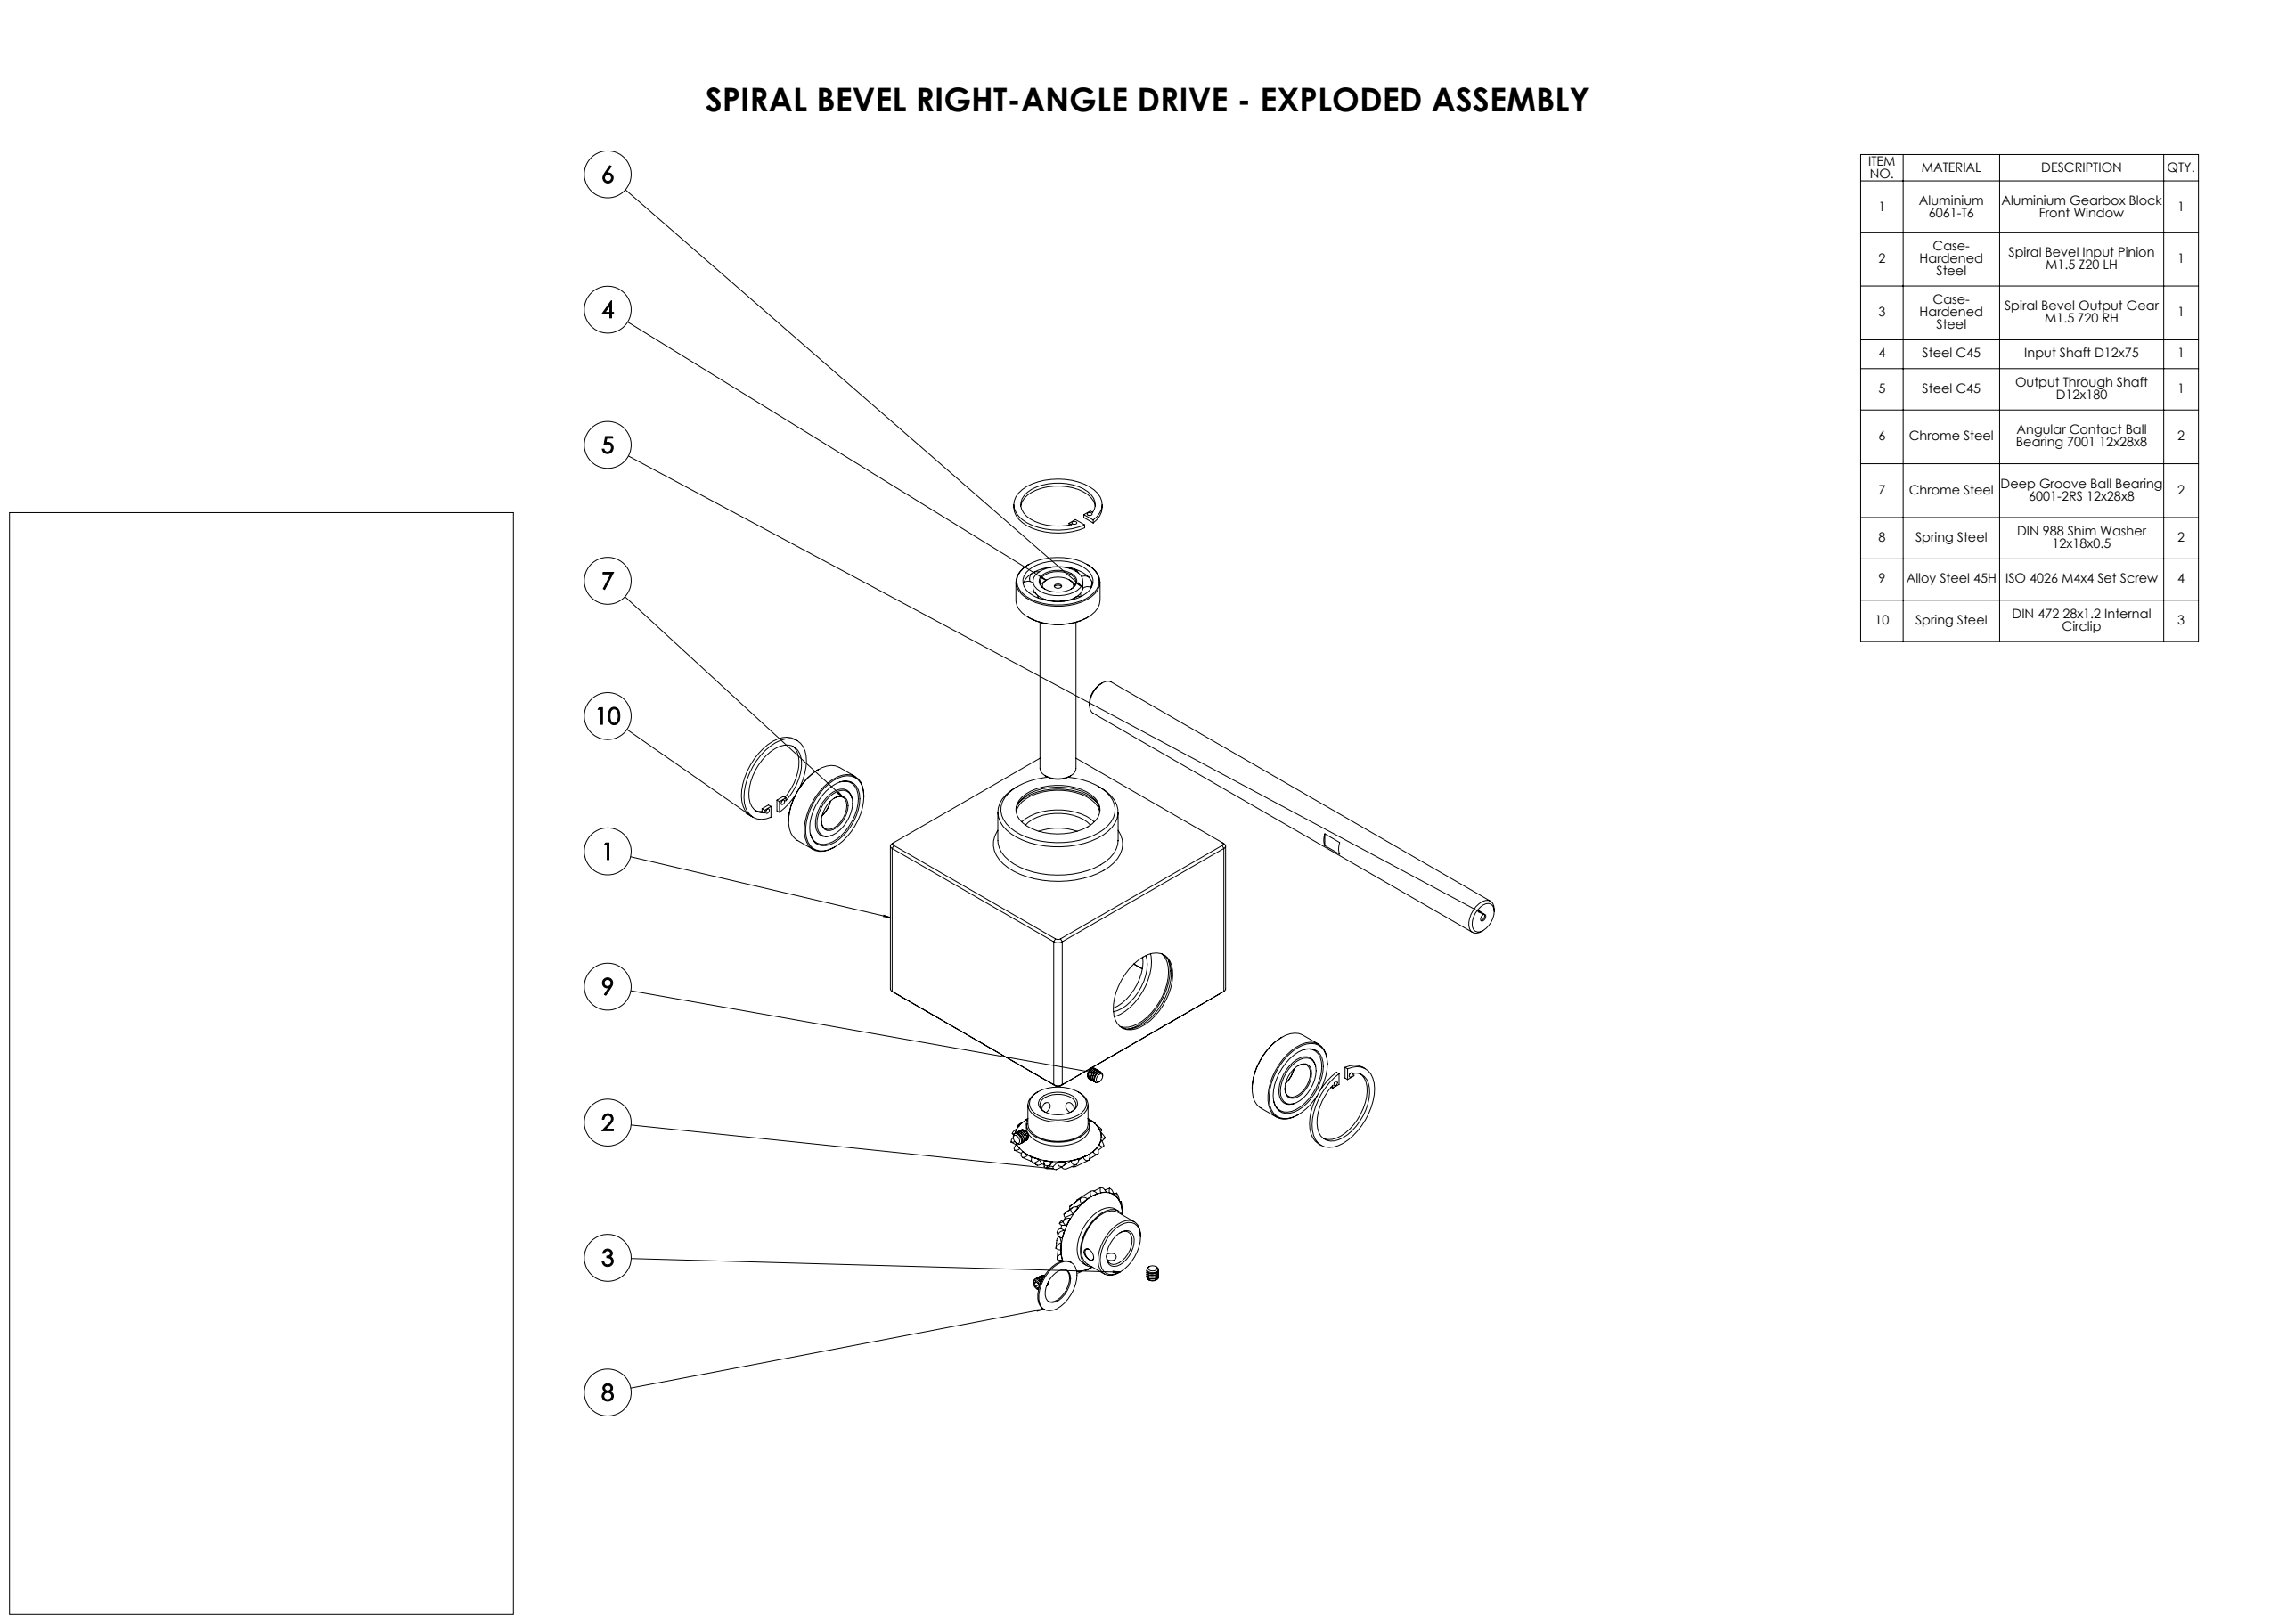
ISO-10303-21;
HEADER;
/* Generated by software containing ST-Developer
 * from STEP Tools, Inc. (www.steptools.com) 
 */

FILE_DESCRIPTION(
/* description */ (''),
/* implementation_level */ '2;1');

FILE_NAME(
/* name */ 'MAS-365',
/* time_stamp */ '2026-10-11T09:12:28-07:00',
/* author */ (''),
/* organization */ (''),
/* preprocessor_version */ 'ST-DEVELOPER v20.2',
/* originating_system */ 'Autodesk Translation Framework v15.15.0.0',
/* authorisation */ '');

FILE_SCHEMA (('AUTOMOTIVE_DESIGN { 1 0 10303 214 3 1 1 }'));
ENDSEC;

DATA;
#10=MECHANICAL_DESIGN_GEOMETRIC_PRESENTATION_REPRESENTATION('',(#647,#648,
#649,#650,#651,#652,#653,#654,#655,#656),#23254);
#11=ITEM_DEFINED_TRANSFORMATION($,$,#7147,#7813);
#12=ITEM_DEFINED_TRANSFORMATION($,$,#7279,#7814);
#13=ITEM_DEFINED_TRANSFORMATION($,$,#7412,#7815);
#14=ITEM_DEFINED_TRANSFORMATION($,$,#7544,#7816);
#15=ITEM_DEFINED_TRANSFORMATION($,$,#7574,#7817);
#16=ITEM_DEFINED_TRANSFORMATION($,$,#7604,#7818);
#17=ITEM_DEFINED_TRANSFORMATION($,$,#7604,#7819);
#18=ITEM_DEFINED_TRANSFORMATION($,$,#7713,#7820);
#19=ITEM_DEFINED_TRANSFORMATION($,$,#7713,#7821);
#20=ITEM_DEFINED_TRANSFORMATION($,$,#7746,#7822);
#21=ITEM_DEFINED_TRANSFORMATION($,$,#7746,#7823);
#22=ITEM_DEFINED_TRANSFORMATION($,$,#7755,#7824);
#23=ITEM_DEFINED_TRANSFORMATION($,$,#7755,#7825);
#24=ITEM_DEFINED_TRANSFORMATION($,$,#7755,#7826);
#25=ITEM_DEFINED_TRANSFORMATION($,$,#7755,#7827);
#26=ITEM_DEFINED_TRANSFORMATION($,$,#7792,#7828);
#27=ITEM_DEFINED_TRANSFORMATION($,$,#7792,#7829);
#28=ITEM_DEFINED_TRANSFORMATION($,$,#7792,#7830);
#29=(
REPRESENTATION_RELATIONSHIP($,$,#23300,#23299)
REPRESENTATION_RELATIONSHIP_WITH_TRANSFORMATION(#11)
SHAPE_REPRESENTATION_RELATIONSHIP()
);
#30=(
REPRESENTATION_RELATIONSHIP($,$,#23301,#23299)
REPRESENTATION_RELATIONSHIP_WITH_TRANSFORMATION(#12)
SHAPE_REPRESENTATION_RELATIONSHIP()
);
#31=(
REPRESENTATION_RELATIONSHIP($,$,#23302,#23299)
REPRESENTATION_RELATIONSHIP_WITH_TRANSFORMATION(#13)
SHAPE_REPRESENTATION_RELATIONSHIP()
);
#32=(
REPRESENTATION_RELATIONSHIP($,$,#23303,#23299)
REPRESENTATION_RELATIONSHIP_WITH_TRANSFORMATION(#14)
SHAPE_REPRESENTATION_RELATIONSHIP()
);
#33=(
REPRESENTATION_RELATIONSHIP($,$,#23304,#23299)
REPRESENTATION_RELATIONSHIP_WITH_TRANSFORMATION(#15)
SHAPE_REPRESENTATION_RELATIONSHIP()
);
#34=(
REPRESENTATION_RELATIONSHIP($,$,#23305,#23299)
REPRESENTATION_RELATIONSHIP_WITH_TRANSFORMATION(#16)
SHAPE_REPRESENTATION_RELATIONSHIP()
);
#35=(
REPRESENTATION_RELATIONSHIP($,$,#23305,#23299)
REPRESENTATION_RELATIONSHIP_WITH_TRANSFORMATION(#17)
SHAPE_REPRESENTATION_RELATIONSHIP()
);
#36=(
REPRESENTATION_RELATIONSHIP($,$,#23306,#23299)
REPRESENTATION_RELATIONSHIP_WITH_TRANSFORMATION(#18)
SHAPE_REPRESENTATION_RELATIONSHIP()
);
#37=(
REPRESENTATION_RELATIONSHIP($,$,#23306,#23299)
REPRESENTATION_RELATIONSHIP_WITH_TRANSFORMATION(#19)
SHAPE_REPRESENTATION_RELATIONSHIP()
);
#38=(
REPRESENTATION_RELATIONSHIP($,$,#23307,#23299)
REPRESENTATION_RELATIONSHIP_WITH_TRANSFORMATION(#20)
SHAPE_REPRESENTATION_RELATIONSHIP()
);
#39=(
REPRESENTATION_RELATIONSHIP($,$,#23307,#23299)
REPRESENTATION_RELATIONSHIP_WITH_TRANSFORMATION(#21)
SHAPE_REPRESENTATION_RELATIONSHIP()
);
#40=(
REPRESENTATION_RELATIONSHIP($,$,#23308,#23299)
REPRESENTATION_RELATIONSHIP_WITH_TRANSFORMATION(#22)
SHAPE_REPRESENTATION_RELATIONSHIP()
);
#41=(
REPRESENTATION_RELATIONSHIP($,$,#23308,#23299)
REPRESENTATION_RELATIONSHIP_WITH_TRANSFORMATION(#23)
SHAPE_REPRESENTATION_RELATIONSHIP()
);
#42=(
REPRESENTATION_RELATIONSHIP($,$,#23308,#23299)
REPRESENTATION_RELATIONSHIP_WITH_TRANSFORMATION(#24)
SHAPE_REPRESENTATION_RELATIONSHIP()
);
#43=(
REPRESENTATION_RELATIONSHIP($,$,#23308,#23299)
REPRESENTATION_RELATIONSHIP_WITH_TRANSFORMATION(#25)
SHAPE_REPRESENTATION_RELATIONSHIP()
);
#44=(
REPRESENTATION_RELATIONSHIP($,$,#23309,#23299)
REPRESENTATION_RELATIONSHIP_WITH_TRANSFORMATION(#26)
SHAPE_REPRESENTATION_RELATIONSHIP()
);
#45=(
REPRESENTATION_RELATIONSHIP($,$,#23309,#23299)
REPRESENTATION_RELATIONSHIP_WITH_TRANSFORMATION(#27)
SHAPE_REPRESENTATION_RELATIONSHIP()
);
#46=(
REPRESENTATION_RELATIONSHIP($,$,#23309,#23299)
REPRESENTATION_RELATIONSHIP_WITH_TRANSFORMATION(#28)
SHAPE_REPRESENTATION_RELATIONSHIP()
);
#47=CONTEXT_DEPENDENT_SHAPE_REPRESENTATION(#29,#23281);
#48=CONTEXT_DEPENDENT_SHAPE_REPRESENTATION(#30,#23282);
#49=CONTEXT_DEPENDENT_SHAPE_REPRESENTATION(#31,#23283);
#50=CONTEXT_DEPENDENT_SHAPE_REPRESENTATION(#32,#23284);
#51=CONTEXT_DEPENDENT_SHAPE_REPRESENTATION(#33,#23285);
#52=CONTEXT_DEPENDENT_SHAPE_REPRESENTATION(#34,#23286);
#53=CONTEXT_DEPENDENT_SHAPE_REPRESENTATION(#35,#23287);
#54=CONTEXT_DEPENDENT_SHAPE_REPRESENTATION(#36,#23288);
#55=CONTEXT_DEPENDENT_SHAPE_REPRESENTATION(#37,#23289);
#56=CONTEXT_DEPENDENT_SHAPE_REPRESENTATION(#38,#23290);
#57=CONTEXT_DEPENDENT_SHAPE_REPRESENTATION(#39,#23291);
#58=CONTEXT_DEPENDENT_SHAPE_REPRESENTATION(#40,#23292);
#59=CONTEXT_DEPENDENT_SHAPE_REPRESENTATION(#41,#23293);
#60=CONTEXT_DEPENDENT_SHAPE_REPRESENTATION(#42,#23294);
#61=CONTEXT_DEPENDENT_SHAPE_REPRESENTATION(#43,#23295);
#62=CONTEXT_DEPENDENT_SHAPE_REPRESENTATION(#44,#23296);
#63=CONTEXT_DEPENDENT_SHAPE_REPRESENTATION(#45,#23297);
#64=CONTEXT_DEPENDENT_SHAPE_REPRESENTATION(#46,#23298);
#65=NEXT_ASSEMBLY_USAGE_OCCURRENCE(
'01_Aluminium_Gearbox_Block_Front_Window:2',
'01_Aluminium_Gearbox_Block_Front_Window:2',
'01_Aluminium_Gearbox_Block_Front_Window:2',#23311,#23312,
'01_Aluminium_Gearbox_Block_Front_Window:2');
#66=NEXT_ASSEMBLY_USAGE_OCCURRENCE(
'02_Spiral_Bevel_Input_Pinion_M1.5_Z20_LH:2',
'02_Spiral_Bevel_Input_Pinion_M1.5_Z20_LH:2',
'02_Spiral_Bevel_Input_Pinion_M1.5_Z20_LH:2',#23311,#23313,
'02_Spiral_Bevel_Input_Pinion_M1.5_Z20_LH:2');
#67=NEXT_ASSEMBLY_USAGE_OCCURRENCE(
'03_Spiral_Bevel_Output_Gear_M1.5_Z20_RH:2',
'03_Spiral_Bevel_Output_Gear_M1.5_Z20_RH:2',
'03_Spiral_Bevel_Output_Gear_M1.5_Z20_RH:2',#23311,#23314,
'03_Spiral_Bevel_Output_Gear_M1.5_Z20_RH:2');
#68=NEXT_ASSEMBLY_USAGE_OCCURRENCE('04_Input_Shaft_D12x75:2',
'04_Input_Shaft_D12x75:2','04_Input_Shaft_D12x75:2',#23311,#23315,
'04_Input_Shaft_D12x75:2');
#69=NEXT_ASSEMBLY_USAGE_OCCURRENCE('05_Output_Through_Shaft_D12x180:2',
'05_Output_Through_Shaft_D12x180:2','05_Output_Through_Shaft_D12x180:2',
#23311,#23316,'05_Output_Through_Shaft_D12x180:2');
#70=NEXT_ASSEMBLY_USAGE_OCCURRENCE(
'06_Angular_Contact_Ball_Bearing_7001_12x28x8:2',
'06_Angular_Contact_Ball_Bearing_7001_12x28x8:2',
'06_Angular_Contact_Ball_Bearing_7001_12x28x8:2',#23311,#23317,
'06_Angular_Contact_Ball_Bearing_7001_12x28x8:2');
#71=NEXT_ASSEMBLY_USAGE_OCCURRENCE(
'06_Angular_Contact_Ball_Bearing_7001_12x28x8:3',
'06_Angular_Contact_Ball_Bearing_7001_12x28x8:3',
'06_Angular_Contact_Ball_Bearing_7001_12x28x8:3',#23311,#23317,
'06_Angular_Contact_Ball_Bearing_7001_12x28x8:3');
#72=NEXT_ASSEMBLY_USAGE_OCCURRENCE(
'07_Deep_Groove_Ball_Bearing_6001-2RS_12x28x8:2',
'07_Deep_Groove_Ball_Bearing_6001-2RS_12x28x8:2',
'07_Deep_Groove_Ball_Bearing_6001-2RS_12x28x8:2',#23311,#23318,
'07_Deep_Groove_Ball_Bearing_6001-2RS_12x28x8:2');
#73=NEXT_ASSEMBLY_USAGE_OCCURRENCE(
'07_Deep_Groove_Ball_Bearing_6001-2RS_12x28x8:3',
'07_Deep_Groove_Ball_Bearing_6001-2RS_12x28x8:3',
'07_Deep_Groove_Ball_Bearing_6001-2RS_12x28x8:3',#23311,#23318,
'07_Deep_Groove_Ball_Bearing_6001-2RS_12x28x8:3');
#74=NEXT_ASSEMBLY_USAGE_OCCURRENCE('08_DIN_988_Shim_Washer_12x18x0.5:2',
'08_DIN_988_Shim_Washer_12x18x0.5:2',
'08_DIN_988_Shim_Washer_12x18x0.5:2',#23311,#23319,
'08_DIN_988_Shim_Washer_12x18x0.5:2');
#75=NEXT_ASSEMBLY_USAGE_OCCURRENCE('08_DIN_988_Shim_Washer_12x18x0.5:3',
'08_DIN_988_Shim_Washer_12x18x0.5:3',
'08_DIN_988_Shim_Washer_12x18x0.5:3',#23311,#23319,
'08_DIN_988_Shim_Washer_12x18x0.5:3');
#76=NEXT_ASSEMBLY_USAGE_OCCURRENCE('09_ISO_4026_M4x4_Set_Screw:2',
'09_ISO_4026_M4x4_Set_Screw:2','09_ISO_4026_M4x4_Set_Screw:2',#23311,#23320,
'09_ISO_4026_M4x4_Set_Screw:2');
#77=NEXT_ASSEMBLY_USAGE_OCCURRENCE('09_ISO_4026_M4x4_Set_Screw:3',
'09_ISO_4026_M4x4_Set_Screw:3','09_ISO_4026_M4x4_Set_Screw:3',#23311,#23320,
'09_ISO_4026_M4x4_Set_Screw:3');
#78=NEXT_ASSEMBLY_USAGE_OCCURRENCE('09_ISO_4026_M4x4_Set_Screw:4',
'09_ISO_4026_M4x4_Set_Screw:4','09_ISO_4026_M4x4_Set_Screw:4',#23311,#23320,
'09_ISO_4026_M4x4_Set_Screw:4');
#79=NEXT_ASSEMBLY_USAGE_OCCURRENCE('09_ISO_4026_M4x4_Set_Screw:5',
'09_ISO_4026_M4x4_Set_Screw:5','09_ISO_4026_M4x4_Set_Screw:5',#23311,#23320,
'09_ISO_4026_M4x4_Set_Screw:5');
#80=NEXT_ASSEMBLY_USAGE_OCCURRENCE(
'10_DIN_472_28x1.2_Internal_Circlip:2',
'10_DIN_472_28x1.2_Internal_Circlip:2',
'10_DIN_472_28x1.2_Internal_Circlip:2',#23311,#23321,
'10_DIN_472_28x1.2_Internal_Circlip:2');
#81=NEXT_ASSEMBLY_USAGE_OCCURRENCE(
'10_DIN_472_28x1.2_Internal_Circlip:3',
'10_DIN_472_28x1.2_Internal_Circlip:3',
'10_DIN_472_28x1.2_Internal_Circlip:3',#23311,#23321,
'10_DIN_472_28x1.2_Internal_Circlip:3');
#82=NEXT_ASSEMBLY_USAGE_OCCURRENCE(
'10_DIN_472_28x1.2_Internal_Circlip:4',
'10_DIN_472_28x1.2_Internal_Circlip:4',
'10_DIN_472_28x1.2_Internal_Circlip:4',#23311,#23321,
'10_DIN_472_28x1.2_Internal_Circlip:4');
#83=SPHERICAL_SURFACE('',#7605,2.38125);
#84=SPHERICAL_SURFACE('',#7635,2.38125);
#85=SPHERICAL_SURFACE('',#7641,2.38125);
#86=SPHERICAL_SURFACE('',#7647,2.38125);
#87=SPHERICAL_SURFACE('',#7653,2.38125);
#88=SPHERICAL_SURFACE('',#7659,2.38125);
#89=SPHERICAL_SURFACE('',#7665,2.38125);
#90=SPHERICAL_SURFACE('',#7671,2.38125);
#91=SPHERICAL_SURFACE('',#7677,2.38125);
#92=SPHERICAL_SURFACE('',#7689,2.38125);
#93=B_SPLINE_SURFACE_WITH_KNOTS('',3,3,((#12095,#12096,#12097,#12098),(#12099,
#12100,#12101,#12102),(#12103,#12104,#12105,#12106),(#12107,#12108,#12109,
#12110),(#12111,#12112,#12113,#12114),(#12115,#12116,#12117,#12118)),
 .UNSPECIFIED.,.F.,.F.,.F.,(4,1,1,4),(4,4),(0.,0.285714285714286,0.571428571428571,
1.),(0.,1.),.UNSPECIFIED.);
#94=B_SPLINE_SURFACE_WITH_KNOTS('',3,3,((#12155,#12156,#12157,#12158),(#12159,
#12160,#12161,#12162),(#12163,#12164,#12165,#12166),(#12167,#12168,#12169,
#12170),(#12171,#12172,#12173,#12174),(#12175,#12176,#12177,#12178)),
 .UNSPECIFIED.,.F.,.F.,.F.,(4,1,1,4),(4,4),(0.,0.285714285714286,0.571428571428571,
1.),(0.,1.),.UNSPECIFIED.);
#95=B_SPLINE_SURFACE_WITH_KNOTS('',3,3,((#12215,#12216,#12217,#12218),(#12219,
#12220,#12221,#12222),(#12223,#12224,#12225,#12226),(#12227,#12228,#12229,
#12230),(#12231,#12232,#12233,#12234),(#12235,#12236,#12237,#12238)),
 .UNSPECIFIED.,.F.,.F.,.F.,(4,1,1,4),(4,4),(0.,0.285714285714286,0.571428571428571,
1.),(0.,1.),.UNSPECIFIED.);
#96=B_SPLINE_SURFACE_WITH_KNOTS('',3,3,((#12275,#12276,#12277,#12278),(#12279,
#12280,#12281,#12282),(#12283,#12284,#12285,#12286),(#12287,#12288,#12289,
#12290),(#12291,#12292,#12293,#12294),(#12295,#12296,#12297,#12298)),
 .UNSPECIFIED.,.F.,.F.,.F.,(4,1,1,4),(4,4),(0.,0.285714285714286,0.571428571428571,
1.),(0.,1.),.UNSPECIFIED.);
#97=B_SPLINE_SURFACE_WITH_KNOTS('',3,3,((#12335,#12336,#12337,#12338),(#12339,
#12340,#12341,#12342),(#12343,#12344,#12345,#12346),(#12347,#12348,#12349,
#12350),(#12351,#12352,#12353,#12354),(#12355,#12356,#12357,#12358)),
 .UNSPECIFIED.,.F.,.F.,.F.,(4,1,1,4),(4,4),(0.,0.285714285714286,0.571428571428571,
1.),(0.,1.),.UNSPECIFIED.);
#98=B_SPLINE_SURFACE_WITH_KNOTS('',3,3,((#12395,#12396,#12397,#12398),(#12399,
#12400,#12401,#12402),(#12403,#12404,#12405,#12406),(#12407,#12408,#12409,
#12410),(#12411,#12412,#12413,#12414),(#12415,#12416,#12417,#12418)),
 .UNSPECIFIED.,.F.,.F.,.F.,(4,1,1,4),(4,4),(0.,0.285714285714286,0.571428571428571,
1.),(0.,1.),.UNSPECIFIED.);
#99=B_SPLINE_SURFACE_WITH_KNOTS('',3,3,((#12455,#12456,#12457,#12458),(#12459,
#12460,#12461,#12462),(#12463,#12464,#12465,#12466),(#12467,#12468,#12469,
#12470),(#12471,#12472,#12473,#12474),(#12475,#12476,#12477,#12478)),
 .UNSPECIFIED.,.F.,.F.,.F.,(4,1,1,4),(4,4),(0.,0.285714285714286,0.571428571428571,
1.),(0.,1.),.UNSPECIFIED.);
#100=B_SPLINE_SURFACE_WITH_KNOTS('',3,3,((#12515,#12516,#12517,#12518),
(#12519,#12520,#12521,#12522),(#12523,#12524,#12525,#12526),(#12527,#12528,
#12529,#12530),(#12531,#12532,#12533,#12534),(#12535,#12536,#12537,#12538)),
 .UNSPECIFIED.,.F.,.F.,.F.,(4,1,1,4),(4,4),(0.,0.285714285714286,0.571428571428571,
1.),(0.,1.),.UNSPECIFIED.);
#101=B_SPLINE_SURFACE_WITH_KNOTS('',3,3,((#12575,#12576,#12577,#12578),
(#12579,#12580,#12581,#12582),(#12583,#12584,#12585,#12586),(#12587,#12588,
#12589,#12590),(#12591,#12592,#12593,#12594),(#12595,#12596,#12597,#12598)),
 .UNSPECIFIED.,.F.,.F.,.F.,(4,1,1,4),(4,4),(0.,0.285714285714286,0.571428571428571,
1.),(0.,1.),.UNSPECIFIED.);
#102=B_SPLINE_SURFACE_WITH_KNOTS('',3,3,((#12635,#12636,#12637,#12638),
(#12639,#12640,#12641,#12642),(#12643,#12644,#12645,#12646),(#12647,#12648,
#12649,#12650),(#12651,#12652,#12653,#12654),(#12655,#12656,#12657,#12658)),
 .UNSPECIFIED.,.F.,.F.,.F.,(4,1,1,4),(4,4),(0.,0.285714285714286,0.571428571428571,
1.),(0.,1.),.UNSPECIFIED.);
#103=B_SPLINE_SURFACE_WITH_KNOTS('',3,3,((#12695,#12696,#12697,#12698),
(#12699,#12700,#12701,#12702),(#12703,#12704,#12705,#12706),(#12707,#12708,
#12709,#12710),(#12711,#12712,#12713,#12714),(#12715,#12716,#12717,#12718)),
 .UNSPECIFIED.,.F.,.F.,.F.,(4,1,1,4),(4,4),(0.,0.285714285714286,0.571428571428571,
1.),(0.,1.),.UNSPECIFIED.);
#104=B_SPLINE_SURFACE_WITH_KNOTS('',3,3,((#12731,#12732,#12733,#12734),
(#12735,#12736,#12737,#12738),(#12739,#12740,#12741,#12742),(#12743,#12744,
#12745,#12746),(#12747,#12748,#12749,#12750),(#12751,#12752,#12753,#12754)),
 .UNSPECIFIED.,.F.,.F.,.F.,(4,1,1,4),(4,4),(0.,0.285714285714286,0.571428571428571,
1.),(0.,1.),.UNSPECIFIED.);
#105=B_SPLINE_SURFACE_WITH_KNOTS('',3,3,((#12791,#12792,#12793,#12794),
(#12795,#12796,#12797,#12798),(#12799,#12800,#12801,#12802),(#12803,#12804,
#12805,#12806),(#12807,#12808,#12809,#12810),(#12811,#12812,#12813,#12814)),
 .UNSPECIFIED.,.F.,.F.,.F.,(4,1,1,4),(4,4),(0.,0.285714285714286,0.571428571428571,
1.),(0.,1.),.UNSPECIFIED.);
#106=B_SPLINE_SURFACE_WITH_KNOTS('',3,3,((#12851,#12852,#12853,#12854),
(#12855,#12856,#12857,#12858),(#12859,#12860,#12861,#12862),(#12863,#12864,
#12865,#12866),(#12867,#12868,#12869,#12870),(#12871,#12872,#12873,#12874)),
 .UNSPECIFIED.,.F.,.F.,.F.,(4,1,1,4),(4,4),(0.,0.285714285714286,0.571428571428571,
1.),(0.,1.),.UNSPECIFIED.);
#107=B_SPLINE_SURFACE_WITH_KNOTS('',3,3,((#12911,#12912,#12913,#12914),
(#12915,#12916,#12917,#12918),(#12919,#12920,#12921,#12922),(#12923,#12924,
#12925,#12926),(#12927,#12928,#12929,#12930),(#12931,#12932,#12933,#12934)),
 .UNSPECIFIED.,.F.,.F.,.F.,(4,1,1,4),(4,4),(0.,0.285714285714286,0.571428571428571,
1.),(0.,1.),.UNSPECIFIED.);
#108=B_SPLINE_SURFACE_WITH_KNOTS('',3,3,((#12971,#12972,#12973,#12974),
(#12975,#12976,#12977,#12978),(#12979,#12980,#12981,#12982),(#12983,#12984,
#12985,#12986),(#12987,#12988,#12989,#12990),(#12991,#12992,#12993,#12994)),
 .UNSPECIFIED.,.F.,.F.,.F.,(4,1,1,4),(4,4),(0.,0.285714285714286,0.571428571428571,
1.),(0.,1.),.UNSPECIFIED.);
#109=B_SPLINE_SURFACE_WITH_KNOTS('',3,3,((#13031,#13032,#13033,#13034),
(#13035,#13036,#13037,#13038),(#13039,#13040,#13041,#13042),(#13043,#13044,
#13045,#13046),(#13047,#13048,#13049,#13050),(#13051,#13052,#13053,#13054)),
 .UNSPECIFIED.,.F.,.F.,.F.,(4,1,1,4),(4,4),(0.,0.285714285714286,0.571428571428571,
1.),(0.,1.),.UNSPECIFIED.);
#110=B_SPLINE_SURFACE_WITH_KNOTS('',3,3,((#13091,#13092,#13093,#13094),
(#13095,#13096,#13097,#13098),(#13099,#13100,#13101,#13102),(#13103,#13104,
#13105,#13106),(#13107,#13108,#13109,#13110),(#13111,#13112,#13113,#13114)),
 .UNSPECIFIED.,.F.,.F.,.F.,(4,1,1,4),(4,4),(0.,0.285714285714286,0.571428571428571,
1.),(0.,1.),.UNSPECIFIED.);
#111=B_SPLINE_SURFACE_WITH_KNOTS('',3,3,((#13151,#13152,#13153,#13154),
(#13155,#13156,#13157,#13158),(#13159,#13160,#13161,#13162),(#13163,#13164,
#13165,#13166),(#13167,#13168,#13169,#13170),(#13171,#13172,#13173,#13174)),
 .UNSPECIFIED.,.F.,.F.,.F.,(4,1,1,4),(4,4),(0.,0.285714285714286,0.571428571428571,
1.),(0.,1.),.UNSPECIFIED.);
#112=B_SPLINE_SURFACE_WITH_KNOTS('',3,3,((#13211,#13212,#13213,#13214),
(#13215,#13216,#13217,#13218),(#13219,#13220,#13221,#13222),(#13223,#13224,
#13225,#13226),(#13227,#13228,#13229,#13230),(#13231,#13232,#13233,#13234)),
 .UNSPECIFIED.,.F.,.F.,.F.,(4,1,1,4),(4,4),(0.,0.285714285714286,0.571428571428571,
1.),(0.,1.),.UNSPECIFIED.);
#113=B_SPLINE_SURFACE_WITH_KNOTS('',3,3,((#13271,#13272,#13273,#13274,#13275,
#13276,#13277,#13278,#13279,#13280),(#13281,#13282,#13283,#13284,#13285,
#13286,#13287,#13288,#13289,#13290),(#13291,#13292,#13293,#13294,#13295,
#13296,#13297,#13298,#13299,#13300),(#13301,#13302,#13303,#13304,#13305,
#13306,#13307,#13308,#13309,#13310),(#13311,#13312,#13313,#13314,#13315,
#13316,#13317,#13318,#13319,#13320),(#13321,#13322,#13323,#13324,#13325,
#13326,#13327,#13328,#13329,#13330),(#13331,#13332,#13333,#13334,#13335,
#13336,#13337,#13338,#13339,#13340),(#13341,#13342,#13343,#13344,#13345,
#13346,#13347,#13348,#13349,#13350),(#13351,#13352,#13353,#13354,#13355,
#13356,#13357,#13358,#13359,#13360),(#13361,#13362,#13363,#13364,#13365,
#13366,#13367,#13368,#13369,#13370),(#13371,#13372,#13373,#13374,#13375,
#13376,#13377,#13378,#13379,#13380)),.UNSPECIFIED.,.F.,.F.,.F.,(4,1,1,1,
1,1,1,1,4),(4,1,1,1,1,1,1,4),(0.,0.142857142857143,0.285714285714286,0.357142857142857,
0.428571428571429,0.571428571428571,0.785714285714286,0.857142857142857,
1.),(0.,0.571428571428571,0.642857142857143,0.714285714285714,0.857142857142857,
0.928571428571429,0.964285714285714,1.),.UNSPECIFIED.);
#114=B_SPLINE_SURFACE_WITH_KNOTS('',3,3,((#14114,#14115,#14116,#14117,#14118,
#14119,#14120,#14121,#14122,#14123),(#14124,#14125,#14126,#14127,#14128,
#14129,#14130,#14131,#14132,#14133),(#14134,#14135,#14136,#14137,#14138,
#14139,#14140,#14141,#14142,#14143),(#14144,#14145,#14146,#14147,#14148,
#14149,#14150,#14151,#14152,#14153),(#14154,#14155,#14156,#14157,#14158,
#14159,#14160,#14161,#14162,#14163),(#14164,#14165,#14166,#14167,#14168,
#14169,#14170,#14171,#14172,#14173),(#14174,#14175,#14176,#14177,#14178,
#14179,#14180,#14181,#14182,#14183),(#14184,#14185,#14186,#14187,#14188,
#14189,#14190,#14191,#14192,#14193),(#14194,#14195,#14196,#14197,#14198,
#14199,#14200,#14201,#14202,#14203),(#14204,#14205,#14206,#14207,#14208,
#14209,#14210,#14211,#14212,#14213),(#14214,#14215,#14216,#14217,#14218,
#14219,#14220,#14221,#14222,#14223)),.UNSPECIFIED.,.F.,.F.,.F.,(4,1,1,1,
1,1,1,1,4),(4,1,1,1,1,1,1,4),(0.,0.142857142857143,0.285714285714286,0.357142857142857,
0.428571428571429,0.571428571428571,0.785714285714286,0.857142857142857,
1.),(0.,0.571428571428571,0.642857142857143,0.714285714285714,0.857142857142857,
0.928571428571429,0.964285714285714,1.),.UNSPECIFIED.);
#115=B_SPLINE_SURFACE_WITH_KNOTS('',3,3,((#14231,#14232,#14233,#14234,#14235,
#14236,#14237,#14238,#14239,#14240),(#14241,#14242,#14243,#14244,#14245,
#14246,#14247,#14248,#14249,#14250),(#14251,#14252,#14253,#14254,#14255,
#14256,#14257,#14258,#14259,#14260),(#14261,#14262,#14263,#14264,#14265,
#14266,#14267,#14268,#14269,#14270),(#14271,#14272,#14273,#14274,#14275,
#14276,#14277,#14278,#14279,#14280),(#14281,#14282,#14283,#14284,#14285,
#14286,#14287,#14288,#14289,#14290),(#14291,#14292,#14293,#14294,#14295,
#14296,#14297,#14298,#14299,#14300),(#14301,#14302,#14303,#14304,#14305,
#14306,#14307,#14308,#14309,#14310),(#14311,#14312,#14313,#14314,#14315,
#14316,#14317,#14318,#14319,#14320),(#14321,#14322,#14323,#14324,#14325,
#14326,#14327,#14328,#14329,#14330),(#14331,#14332,#14333,#14334,#14335,
#14336,#14337,#14338,#14339,#14340)),.UNSPECIFIED.,.F.,.F.,.F.,(4,1,1,1,
1,1,1,1,4),(4,1,1,1,1,1,1,4),(0.,0.142857142857143,0.285714285714286,0.357142857142857,
0.428571428571429,0.571428571428571,0.785714285714286,0.857142857142857,
1.),(0.,0.571428571428571,0.642857142857143,0.714285714285714,0.857142857142857,
0.928571428571429,0.964285714285714,1.),.UNSPECIFIED.);
#116=B_SPLINE_SURFACE_WITH_KNOTS('',3,3,((#14348,#14349,#14350,#14351),
(#14352,#14353,#14354,#14355),(#14356,#14357,#14358,#14359),(#14360,#14361,
#14362,#14363),(#14364,#14365,#14366,#14367),(#14368,#14369,#14370,#14371),
(#14372,#14373,#14374,#14375),(#14376,#14377,#14378,#14379),(#14380,#14381,
#14382,#14383),(#14384,#14385,#14386,#14387),(#14388,#14389,#14390,#14391),
(#14392,#14393,#14394,#14395)),.UNSPECIFIED.,.F.,.F.,.F.,(4,1,1,1,1,1,1,
1,1,4),(4,4),(0.,0.142857142857143,0.285714285714286,0.321428571428571,
0.357142857142857,0.428571428571429,0.571428571428571,0.785714285714286,
0.857142857142857,1.),(0.,1.),.UNSPECIFIED.);
#117=B_SPLINE_SURFACE_WITH_KNOTS('',3,3,((#14403,#14404,#14405,#14406),
(#14407,#14408,#14409,#14410),(#14411,#14412,#14413,#14414),(#14415,#14416,
#14417,#14418),(#14419,#14420,#14421,#14422),(#14423,#14424,#14425,#14426),
(#14427,#14428,#14429,#14430),(#14431,#14432,#14433,#14434),(#14435,#14436,
#14437,#14438),(#14439,#14440,#14441,#14442),(#14443,#14444,#14445,#14446),
(#14447,#14448,#14449,#14450)),.UNSPECIFIED.,.F.,.F.,.F.,(4,1,1,1,1,1,1,
1,1,4),(4,4),(0.,0.142857142857143,0.285714285714286,0.321428571428571,
0.357142857142857,0.428571428571429,0.571428571428571,0.785714285714286,
0.857142857142857,1.),(0.,1.),.UNSPECIFIED.);
#118=B_SPLINE_SURFACE_WITH_KNOTS('',3,3,((#14458,#14459,#14460,#14461,#14462,
#14463,#14464,#14465,#14466,#14467),(#14468,#14469,#14470,#14471,#14472,
#14473,#14474,#14475,#14476,#14477),(#14478,#14479,#14480,#14481,#14482,
#14483,#14484,#14485,#14486,#14487),(#14488,#14489,#14490,#14491,#14492,
#14493,#14494,#14495,#14496,#14497),(#14498,#14499,#14500,#14501,#14502,
#14503,#14504,#14505,#14506,#14507),(#14508,#14509,#14510,#14511,#14512,
#14513,#14514,#14515,#14516,#14517),(#14518,#14519,#14520,#14521,#14522,
#14523,#14524,#14525,#14526,#14527),(#14528,#14529,#14530,#14531,#14532,
#14533,#14534,#14535,#14536,#14537),(#14538,#14539,#14540,#14541,#14542,
#14543,#14544,#14545,#14546,#14547),(#14548,#14549,#14550,#14551,#14552,
#14553,#14554,#14555,#14556,#14557),(#14558,#14559,#14560,#14561,#14562,
#14563,#14564,#14565,#14566,#14567)),.UNSPECIFIED.,.F.,.F.,.F.,(4,1,1,1,
1,1,1,1,4),(4,1,1,1,1,1,1,4),(0.,0.142857142857143,0.285714285714286,0.357142857142857,
0.428571428571429,0.571428571428571,0.785714285714286,0.857142857142857,
1.),(0.,0.571428571428571,0.642857142857143,0.714285714285714,0.857142857142857,
0.928571428571429,0.964285714285714,1.),.UNSPECIFIED.);
#119=B_SPLINE_SURFACE_WITH_KNOTS('',3,3,((#14575,#14576,#14577,#14578,#14579,
#14580,#14581,#14582,#14583,#14584),(#14585,#14586,#14587,#14588,#14589,
#14590,#14591,#14592,#14593,#14594),(#14595,#14596,#14597,#14598,#14599,
#14600,#14601,#14602,#14603,#14604),(#14605,#14606,#14607,#14608,#14609,
#14610,#14611,#14612,#14613,#14614),(#14615,#14616,#14617,#14618,#14619,
#14620,#14621,#14622,#14623,#14624),(#14625,#14626,#14627,#14628,#14629,
#14630,#14631,#14632,#14633,#14634),(#14635,#14636,#14637,#14638,#14639,
#14640,#14641,#14642,#14643,#14644),(#14645,#14646,#14647,#14648,#14649,
#14650,#14651,#14652,#14653,#14654),(#14655,#14656,#14657,#14658,#14659,
#14660,#14661,#14662,#14663,#14664),(#14665,#14666,#14667,#14668,#14669,
#14670,#14671,#14672,#14673,#14674),(#14675,#14676,#14677,#14678,#14679,
#14680,#14681,#14682,#14683,#14684)),.UNSPECIFIED.,.F.,.F.,.F.,(4,1,1,1,
1,1,1,1,4),(4,1,1,1,1,1,1,4),(0.,0.142857142857143,0.285714285714286,0.357142857142857,
0.428571428571429,0.571428571428571,0.785714285714286,0.857142857142857,
1.),(0.,0.571428571428571,0.642857142857143,0.714285714285714,0.857142857142857,
0.928571428571429,0.964285714285714,1.),.UNSPECIFIED.);
#120=B_SPLINE_SURFACE_WITH_KNOTS('',3,3,((#14692,#14693,#14694,#14695,#14696,
#14697,#14698,#14699,#14700,#14701),(#14702,#14703,#14704,#14705,#14706,
#14707,#14708,#14709,#14710,#14711),(#14712,#14713,#14714,#14715,#14716,
#14717,#14718,#14719,#14720,#14721),(#14722,#14723,#14724,#14725,#14726,
#14727,#14728,#14729,#14730,#14731),(#14732,#14733,#14734,#14735,#14736,
#14737,#14738,#14739,#14740,#14741),(#14742,#14743,#14744,#14745,#14746,
#14747,#14748,#14749,#14750,#14751),(#14752,#14753,#14754,#14755,#14756,
#14757,#14758,#14759,#14760,#14761),(#14762,#14763,#14764,#14765,#14766,
#14767,#14768,#14769,#14770,#14771),(#14772,#14773,#14774,#14775,#14776,
#14777,#14778,#14779,#14780,#14781),(#14782,#14783,#14784,#14785,#14786,
#14787,#14788,#14789,#14790,#14791),(#14792,#14793,#14794,#14795,#14796,
#14797,#14798,#14799,#14800,#14801)),.UNSPECIFIED.,.F.,.F.,.F.,(4,1,1,1,
1,1,1,1,4),(4,1,1,1,1,1,1,4),(0.,0.142857142857143,0.285714285714286,0.357142857142857,
0.428571428571429,0.571428571428571,0.785714285714286,0.857142857142857,
1.),(0.,0.571428571428571,0.642857142857143,0.714285714285714,0.857142857142857,
0.928571428571429,0.964285714285714,1.),.UNSPECIFIED.);
#121=B_SPLINE_SURFACE_WITH_KNOTS('',3,3,((#14809,#14810,#14811,#14812),
(#14813,#14814,#14815,#14816),(#14817,#14818,#14819,#14820),(#14821,#14822,
#14823,#14824),(#14825,#14826,#14827,#14828),(#14829,#14830,#14831,#14832),
(#14833,#14834,#14835,#14836),(#14837,#14838,#14839,#14840),(#14841,#14842,
#14843,#14844),(#14845,#14846,#14847,#14848),(#14849,#14850,#14851,#14852),
(#14853,#14854,#14855,#14856)),.UNSPECIFIED.,.F.,.F.,.F.,(4,1,1,1,1,1,1,
1,1,4),(4,4),(0.,0.142857142857143,0.285714285714286,0.321428571428571,
0.357142857142857,0.428571428571429,0.571428571428571,0.785714285714286,
0.857142857142857,1.),(0.,1.),.UNSPECIFIED.);
#122=B_SPLINE_SURFACE_WITH_KNOTS('',3,3,((#14864,#14865,#14866,#14867),
(#14868,#14869,#14870,#14871),(#14872,#14873,#14874,#14875),(#14876,#14877,
#14878,#14879),(#14880,#14881,#14882,#14883),(#14884,#14885,#14886,#14887),
(#14888,#14889,#14890,#14891),(#14892,#14893,#14894,#14895),(#14896,#14897,
#14898,#14899),(#14900,#14901,#14902,#14903),(#14904,#14905,#14906,#14907),
(#14908,#14909,#14910,#14911)),.UNSPECIFIED.,.F.,.F.,.F.,(4,1,1,1,1,1,1,
1,1,4),(4,4),(0.,0.142857142857143,0.285714285714286,0.321428571428571,
0.357142857142857,0.428571428571429,0.571428571428571,0.785714285714286,
0.857142857142857,1.),(0.,1.),.UNSPECIFIED.);
#123=B_SPLINE_SURFACE_WITH_KNOTS('',3,3,((#14919,#14920,#14921,#14922,#14923,
#14924,#14925,#14926,#14927,#14928),(#14929,#14930,#14931,#14932,#14933,
#14934,#14935,#14936,#14937,#14938),(#14939,#14940,#14941,#14942,#14943,
#14944,#14945,#14946,#14947,#14948),(#14949,#14950,#14951,#14952,#14953,
#14954,#14955,#14956,#14957,#14958),(#14959,#14960,#14961,#14962,#14963,
#14964,#14965,#14966,#14967,#14968),(#14969,#14970,#14971,#14972,#14973,
#14974,#14975,#14976,#14977,#14978),(#14979,#14980,#14981,#14982,#14983,
#14984,#14985,#14986,#14987,#14988),(#14989,#14990,#14991,#14992,#14993,
#14994,#14995,#14996,#14997,#14998),(#14999,#15000,#15001,#15002,#15003,
#15004,#15005,#15006,#15007,#15008),(#15009,#15010,#15011,#15012,#15013,
#15014,#15015,#15016,#15017,#15018),(#15019,#15020,#15021,#15022,#15023,
#15024,#15025,#15026,#15027,#15028)),.UNSPECIFIED.,.F.,.F.,.F.,(4,1,1,1,
1,1,1,1,4),(4,1,1,1,1,1,1,4),(0.,0.142857142857143,0.285714285714286,0.357142857142857,
0.428571428571429,0.571428571428571,0.785714285714286,0.857142857142857,
1.),(0.,0.571428571428571,0.642857142857143,0.714285714285714,0.857142857142857,
0.928571428571429,0.964285714285714,1.),.UNSPECIFIED.);
#124=B_SPLINE_SURFACE_WITH_KNOTS('',3,3,((#15036,#15037,#15038,#15039,#15040,
#15041,#15042,#15043,#15044,#15045),(#15046,#15047,#15048,#15049,#15050,
#15051,#15052,#15053,#15054,#15055),(#15056,#15057,#15058,#15059,#15060,
#15061,#15062,#15063,#15064,#15065),(#15066,#15067,#15068,#15069,#15070,
#15071,#15072,#15073,#15074,#15075),(#15076,#15077,#15078,#15079,#15080,
#15081,#15082,#15083,#15084,#15085),(#15086,#15087,#15088,#15089,#15090,
#15091,#15092,#15093,#15094,#15095),(#15096,#15097,#15098,#15099,#15100,
#15101,#15102,#15103,#15104,#15105),(#15106,#15107,#15108,#15109,#15110,
#15111,#15112,#15113,#15114,#15115),(#15116,#15117,#15118,#15119,#15120,
#15121,#15122,#15123,#15124,#15125),(#15126,#15127,#15128,#15129,#15130,
#15131,#15132,#15133,#15134,#15135),(#15136,#15137,#15138,#15139,#15140,
#15141,#15142,#15143,#15144,#15145)),.UNSPECIFIED.,.F.,.F.,.F.,(4,1,1,1,
1,1,1,1,4),(4,1,1,1,1,1,1,4),(0.,0.142857142857143,0.285714285714286,0.357142857142857,
0.428571428571429,0.571428571428571,0.785714285714286,0.857142857142857,
1.),(0.,0.571428571428571,0.642857142857143,0.714285714285714,0.857142857142857,
0.928571428571429,0.964285714285714,1.),.UNSPECIFIED.);
#125=B_SPLINE_SURFACE_WITH_KNOTS('',3,3,((#15153,#15154,#15155,#15156,#15157,
#15158,#15159,#15160,#15161,#15162),(#15163,#15164,#15165,#15166,#15167,
#15168,#15169,#15170,#15171,#15172),(#15173,#15174,#15175,#15176,#15177,
#15178,#15179,#15180,#15181,#15182),(#15183,#15184,#15185,#15186,#15187,
#15188,#15189,#15190,#15191,#15192),(#15193,#15194,#15195,#15196,#15197,
#15198,#15199,#15200,#15201,#15202),(#15203,#15204,#15205,#15206,#15207,
#15208,#15209,#15210,#15211,#15212),(#15213,#15214,#15215,#15216,#15217,
#15218,#15219,#15220,#15221,#15222),(#15223,#15224,#15225,#15226,#15227,
#15228,#15229,#15230,#15231,#15232),(#15233,#15234,#15235,#15236,#15237,
#15238,#15239,#15240,#15241,#15242),(#15243,#15244,#15245,#15246,#15247,
#15248,#15249,#15250,#15251,#15252),(#15253,#15254,#15255,#15256,#15257,
#15258,#15259,#15260,#15261,#15262)),.UNSPECIFIED.,.F.,.F.,.F.,(4,1,1,1,
1,1,1,1,4),(4,1,1,1,1,1,1,4),(0.,0.142857142857143,0.285714285714286,0.357142857142857,
0.428571428571429,0.571428571428571,0.785714285714286,0.857142857142857,
1.),(0.,0.571428571428571,0.642857142857143,0.714285714285714,0.857142857142857,
0.928571428571429,0.964285714285714,1.),.UNSPECIFIED.);
#126=B_SPLINE_SURFACE_WITH_KNOTS('',3,3,((#15270,#15271,#15272,#15273),
(#15274,#15275,#15276,#15277),(#15278,#15279,#15280,#15281),(#15282,#15283,
#15284,#15285),(#15286,#15287,#15288,#15289),(#15290,#15291,#15292,#15293),
(#15294,#15295,#15296,#15297),(#15298,#15299,#15300,#15301),(#15302,#15303,
#15304,#15305),(#15306,#15307,#15308,#15309),(#15310,#15311,#15312,#15313),
(#15314,#15315,#15316,#15317)),.UNSPECIFIED.,.F.,.F.,.F.,(4,1,1,1,1,1,1,
1,1,4),(4,4),(0.,0.142857142857143,0.285714285714286,0.321428571428571,
0.357142857142857,0.428571428571429,0.571428571428571,0.785714285714286,
0.857142857142857,1.),(0.,1.),.UNSPECIFIED.);
#127=B_SPLINE_SURFACE_WITH_KNOTS('',3,3,((#15325,#15326,#15327,#15328),
(#15329,#15330,#15331,#15332),(#15333,#15334,#15335,#15336),(#15337,#15338,
#15339,#15340),(#15341,#15342,#15343,#15344),(#15345,#15346,#15347,#15348),
(#15349,#15350,#15351,#15352),(#15353,#15354,#15355,#15356),(#15357,#15358,
#15359,#15360),(#15361,#15362,#15363,#15364),(#15365,#15366,#15367,#15368),
(#15369,#15370,#15371,#15372)),.UNSPECIFIED.,.F.,.F.,.F.,(4,1,1,1,1,1,1,
1,1,4),(4,4),(0.,0.142857142857143,0.285714285714286,0.321428571428571,
0.357142857142857,0.428571428571429,0.571428571428571,0.785714285714286,
0.857142857142857,1.),(0.,1.),.UNSPECIFIED.);
#128=B_SPLINE_SURFACE_WITH_KNOTS('',3,3,((#15380,#15381,#15382,#15383,#15384,
#15385,#15386,#15387,#15388,#15389),(#15390,#15391,#15392,#15393,#15394,
#15395,#15396,#15397,#15398,#15399),(#15400,#15401,#15402,#15403,#15404,
#15405,#15406,#15407,#15408,#15409),(#15410,#15411,#15412,#15413,#15414,
#15415,#15416,#15417,#15418,#15419),(#15420,#15421,#15422,#15423,#15424,
#15425,#15426,#15427,#15428,#15429),(#15430,#15431,#15432,#15433,#15434,
#15435,#15436,#15437,#15438,#15439),(#15440,#15441,#15442,#15443,#15444,
#15445,#15446,#15447,#15448,#15449),(#15450,#15451,#15452,#15453,#15454,
#15455,#15456,#15457,#15458,#15459),(#15460,#15461,#15462,#15463,#15464,
#15465,#15466,#15467,#15468,#15469),(#15470,#15471,#15472,#15473,#15474,
#15475,#15476,#15477,#15478,#15479),(#15480,#15481,#15482,#15483,#15484,
#15485,#15486,#15487,#15488,#15489)),.UNSPECIFIED.,.F.,.F.,.F.,(4,1,1,1,
1,1,1,1,4),(4,1,1,1,1,1,1,4),(0.,0.142857142857143,0.285714285714286,0.357142857142857,
0.428571428571429,0.571428571428571,0.785714285714286,0.857142857142857,
1.),(0.,0.571428571428571,0.642857142857143,0.714285714285714,0.857142857142857,
0.928571428571429,0.964285714285714,1.),.UNSPECIFIED.);
#129=B_SPLINE_SURFACE_WITH_KNOTS('',3,3,((#15497,#15498,#15499,#15500,#15501,
#15502,#15503,#15504,#15505,#15506),(#15507,#15508,#15509,#15510,#15511,
#15512,#15513,#15514,#15515,#15516),(#15517,#15518,#15519,#15520,#15521,
#15522,#15523,#15524,#15525,#15526),(#15527,#15528,#15529,#15530,#15531,
#15532,#15533,#15534,#15535,#15536),(#15537,#15538,#15539,#15540,#15541,
#15542,#15543,#15544,#15545,#15546),(#15547,#15548,#15549,#15550,#15551,
#15552,#15553,#15554,#15555,#15556),(#15557,#15558,#15559,#15560,#15561,
#15562,#15563,#15564,#15565,#15566),(#15567,#15568,#15569,#15570,#15571,
#15572,#15573,#15574,#15575,#15576),(#15577,#15578,#15579,#15580,#15581,
#15582,#15583,#15584,#15585,#15586),(#15587,#15588,#15589,#15590,#15591,
#15592,#15593,#15594,#15595,#15596),(#15597,#15598,#15599,#15600,#15601,
#15602,#15603,#15604,#15605,#15606)),.UNSPECIFIED.,.F.,.F.,.F.,(4,1,1,1,
1,1,1,1,4),(4,1,1,1,1,1,1,4),(0.,0.142857142857143,0.285714285714286,0.357142857142857,
0.428571428571429,0.571428571428571,0.785714285714286,0.857142857142857,
1.),(0.,0.571428571428571,0.642857142857143,0.714285714285714,0.857142857142857,
0.928571428571429,0.964285714285714,1.),.UNSPECIFIED.);
#130=B_SPLINE_SURFACE_WITH_KNOTS('',3,3,((#15614,#15615,#15616,#15617,#15618,
#15619,#15620,#15621,#15622,#15623),(#15624,#15625,#15626,#15627,#15628,
#15629,#15630,#15631,#15632,#15633),(#15634,#15635,#15636,#15637,#15638,
#15639,#15640,#15641,#15642,#15643),(#15644,#15645,#15646,#15647,#15648,
#15649,#15650,#15651,#15652,#15653),(#15654,#15655,#15656,#15657,#15658,
#15659,#15660,#15661,#15662,#15663),(#15664,#15665,#15666,#15667,#15668,
#15669,#15670,#15671,#15672,#15673),(#15674,#15675,#15676,#15677,#15678,
#15679,#15680,#15681,#15682,#15683),(#15684,#15685,#15686,#15687,#15688,
#15689,#15690,#15691,#15692,#15693),(#15694,#15695,#15696,#15697,#15698,
#15699,#15700,#15701,#15702,#15703),(#15704,#15705,#15706,#15707,#15708,
#15709,#15710,#15711,#15712,#15713),(#15714,#15715,#15716,#15717,#15718,
#15719,#15720,#15721,#15722,#15723)),.UNSPECIFIED.,.F.,.F.,.F.,(4,1,1,1,
1,1,1,1,4),(4,1,1,1,1,1,1,4),(0.,0.142857142857143,0.285714285714286,0.357142857142857,
0.428571428571429,0.571428571428571,0.785714285714286,0.857142857142857,
1.),(0.,0.571428571428571,0.642857142857143,0.714285714285714,0.857142857142857,
0.928571428571429,0.964285714285714,1.),.UNSPECIFIED.);
#131=B_SPLINE_SURFACE_WITH_KNOTS('',3,3,((#15731,#15732,#15733,#15734),
(#15735,#15736,#15737,#15738),(#15739,#15740,#15741,#15742),(#15743,#15744,
#15745,#15746),(#15747,#15748,#15749,#15750),(#15751,#15752,#15753,#15754),
(#15755,#15756,#15757,#15758),(#15759,#15760,#15761,#15762),(#15763,#15764,
#15765,#15766),(#15767,#15768,#15769,#15770),(#15771,#15772,#15773,#15774),
(#15775,#15776,#15777,#15778)),.UNSPECIFIED.,.F.,.F.,.F.,(4,1,1,1,1,1,1,
1,1,4),(4,4),(0.,0.142857142857143,0.285714285714286,0.321428571428571,
0.357142857142857,0.428571428571429,0.571428571428571,0.785714285714286,
0.857142857142857,1.),(0.,1.),.UNSPECIFIED.);
#132=B_SPLINE_SURFACE_WITH_KNOTS('',3,3,((#15786,#15787,#15788,#15789),
(#15790,#15791,#15792,#15793),(#15794,#15795,#15796,#15797),(#15798,#15799,
#15800,#15801),(#15802,#15803,#15804,#15805),(#15806,#15807,#15808,#15809),
(#15810,#15811,#15812,#15813),(#15814,#15815,#15816,#15817),(#15818,#15819,
#15820,#15821),(#15822,#15823,#15824,#15825),(#15826,#15827,#15828,#15829),
(#15830,#15831,#15832,#15833)),.UNSPECIFIED.,.F.,.F.,.F.,(4,1,1,1,1,1,1,
1,1,4),(4,4),(0.,0.142857142857143,0.285714285714286,0.321428571428571,
0.357142857142857,0.428571428571429,0.571428571428571,0.785714285714286,
0.857142857142857,1.),(0.,1.),.UNSPECIFIED.);
#133=B_SPLINE_SURFACE_WITH_KNOTS('',3,3,((#18119,#18120,#18121,#18122),
(#18123,#18124,#18125,#18126),(#18127,#18128,#18129,#18130),(#18131,#18132,
#18133,#18134),(#18135,#18136,#18137,#18138),(#18139,#18140,#18141,#18142)),
 .UNSPECIFIED.,.F.,.F.,.F.,(4,1,1,4),(4,4),(0.,0.285714285714286,0.571428571428571,
1.),(0.,1.),.UNSPECIFIED.);
#134=B_SPLINE_SURFACE_WITH_KNOTS('',3,3,((#18179,#18180,#18181,#18182),
(#18183,#18184,#18185,#18186),(#18187,#18188,#18189,#18190),(#18191,#18192,
#18193,#18194),(#18195,#18196,#18197,#18198),(#18199,#18200,#18201,#18202)),
 .UNSPECIFIED.,.F.,.F.,.F.,(4,1,1,4),(4,4),(0.,0.285714285714286,0.571428571428571,
1.),(0.,1.),.UNSPECIFIED.);
#135=B_SPLINE_SURFACE_WITH_KNOTS('',3,3,((#18239,#18240,#18241,#18242),
(#18243,#18244,#18245,#18246),(#18247,#18248,#18249,#18250),(#18251,#18252,
#18253,#18254),(#18255,#18256,#18257,#18258),(#18259,#18260,#18261,#18262)),
 .UNSPECIFIED.,.F.,.F.,.F.,(4,1,1,4),(4,4),(0.,0.285714285714286,0.571428571428571,
1.),(0.,1.),.UNSPECIFIED.);
#136=B_SPLINE_SURFACE_WITH_KNOTS('',3,3,((#18299,#18300,#18301,#18302),
(#18303,#18304,#18305,#18306),(#18307,#18308,#18309,#18310),(#18311,#18312,
#18313,#18314),(#18315,#18316,#18317,#18318),(#18319,#18320,#18321,#18322)),
 .UNSPECIFIED.,.F.,.F.,.F.,(4,1,1,4),(4,4),(0.,0.285714285714286,0.571428571428571,
1.),(0.,1.),.UNSPECIFIED.);
#137=B_SPLINE_SURFACE_WITH_KNOTS('',3,3,((#18359,#18360,#18361,#18362),
(#18363,#18364,#18365,#18366),(#18367,#18368,#18369,#18370),(#18371,#18372,
#18373,#18374),(#18375,#18376,#18377,#18378),(#18379,#18380,#18381,#18382)),
 .UNSPECIFIED.,.F.,.F.,.F.,(4,1,1,4),(4,4),(0.,0.285714285714286,0.571428571428571,
1.),(0.,1.),.UNSPECIFIED.);
#138=B_SPLINE_SURFACE_WITH_KNOTS('',3,3,((#18419,#18420,#18421,#18422),
(#18423,#18424,#18425,#18426),(#18427,#18428,#18429,#18430),(#18431,#18432,
#18433,#18434),(#18435,#18436,#18437,#18438),(#18439,#18440,#18441,#18442)),
 .UNSPECIFIED.,.F.,.F.,.F.,(4,1,1,4),(4,4),(0.,0.285714285714286,0.571428571428571,
1.),(0.,1.),.UNSPECIFIED.);
#139=B_SPLINE_SURFACE_WITH_KNOTS('',3,3,((#18479,#18480,#18481,#18482),
(#18483,#18484,#18485,#18486),(#18487,#18488,#18489,#18490),(#18491,#18492,
#18493,#18494),(#18495,#18496,#18497,#18498),(#18499,#18500,#18501,#18502)),
 .UNSPECIFIED.,.F.,.F.,.F.,(4,1,1,4),(4,4),(0.,0.285714285714286,0.571428571428571,
1.),(0.,1.),.UNSPECIFIED.);
#140=B_SPLINE_SURFACE_WITH_KNOTS('',3,3,((#18539,#18540,#18541,#18542),
(#18543,#18544,#18545,#18546),(#18547,#18548,#18549,#18550),(#18551,#18552,
#18553,#18554),(#18555,#18556,#18557,#18558),(#18559,#18560,#18561,#18562)),
 .UNSPECIFIED.,.F.,.F.,.F.,(4,1,1,4),(4,4),(0.,0.285714285714286,0.571428571428571,
1.),(0.,1.),.UNSPECIFIED.);
#141=B_SPLINE_SURFACE_WITH_KNOTS('',3,3,((#18599,#18600,#18601,#18602),
(#18603,#18604,#18605,#18606),(#18607,#18608,#18609,#18610),(#18611,#18612,
#18613,#18614),(#18615,#18616,#18617,#18618),(#18619,#18620,#18621,#18622)),
 .UNSPECIFIED.,.F.,.F.,.F.,(4,1,1,4),(4,4),(0.,0.285714285714286,0.571428571428571,
1.),(0.,1.),.UNSPECIFIED.);
#142=B_SPLINE_SURFACE_WITH_KNOTS('',3,3,((#18659,#18660,#18661,#18662),
(#18663,#18664,#18665,#18666),(#18667,#18668,#18669,#18670),(#18671,#18672,
#18673,#18674),(#18675,#18676,#18677,#18678),(#18679,#18680,#18681,#18682)),
 .UNSPECIFIED.,.F.,.F.,.F.,(4,1,1,4),(4,4),(0.,0.285714285714286,0.571428571428571,
1.),(0.,1.),.UNSPECIFIED.);
#143=B_SPLINE_SURFACE_WITH_KNOTS('',3,3,((#18719,#18720,#18721,#18722),
(#18723,#18724,#18725,#18726),(#18727,#18728,#18729,#18730),(#18731,#18732,
#18733,#18734),(#18735,#18736,#18737,#18738),(#18739,#18740,#18741,#18742)),
 .UNSPECIFIED.,.F.,.F.,.F.,(4,1,1,4),(4,4),(0.,0.285714285714286,0.571428571428571,
1.),(0.,1.),.UNSPECIFIED.);
#144=B_SPLINE_SURFACE_WITH_KNOTS('',3,3,((#18779,#18780,#18781,#18782),
(#18783,#18784,#18785,#18786),(#18787,#18788,#18789,#18790),(#18791,#18792,
#18793,#18794),(#18795,#18796,#18797,#18798),(#18799,#18800,#18801,#18802)),
 .UNSPECIFIED.,.F.,.F.,.F.,(4,1,1,4),(4,4),(0.,0.285714285714286,0.571428571428571,
1.),(0.,1.),.UNSPECIFIED.);
#145=B_SPLINE_SURFACE_WITH_KNOTS('',3,3,((#18839,#18840,#18841,#18842),
(#18843,#18844,#18845,#18846),(#18847,#18848,#18849,#18850),(#18851,#18852,
#18853,#18854),(#18855,#18856,#18857,#18858),(#18859,#18860,#18861,#18862)),
 .UNSPECIFIED.,.F.,.F.,.F.,(4,1,1,4),(4,4),(0.,0.285714285714286,0.571428571428571,
1.),(0.,1.),.UNSPECIFIED.);
#146=B_SPLINE_SURFACE_WITH_KNOTS('',3,3,((#18899,#18900,#18901,#18902),
(#18903,#18904,#18905,#18906),(#18907,#18908,#18909,#18910),(#18911,#18912,
#18913,#18914),(#18915,#18916,#18917,#18918),(#18919,#18920,#18921,#18922)),
 .UNSPECIFIED.,.F.,.F.,.F.,(4,1,1,4),(4,4),(0.,0.285714285714286,0.571428571428571,
1.),(0.,1.),.UNSPECIFIED.);
#147=B_SPLINE_SURFACE_WITH_KNOTS('',3,3,((#18959,#18960,#18961,#18962),
(#18963,#18964,#18965,#18966),(#18967,#18968,#18969,#18970),(#18971,#18972,
#18973,#18974),(#18975,#18976,#18977,#18978),(#18979,#18980,#18981,#18982)),
 .UNSPECIFIED.,.F.,.F.,.F.,(4,1,1,4),(4,4),(0.,0.285714285714286,0.571428571428571,
1.),(0.,1.),.UNSPECIFIED.);
#148=B_SPLINE_SURFACE_WITH_KNOTS('',3,3,((#19019,#19020,#19021,#19022),
(#19023,#19024,#19025,#19026),(#19027,#19028,#19029,#19030),(#19031,#19032,
#19033,#19034),(#19035,#19036,#19037,#19038),(#19039,#19040,#19041,#19042)),
 .UNSPECIFIED.,.F.,.F.,.F.,(4,1,1,4),(4,4),(0.,0.285714285714286,0.571428571428571,
1.),(0.,1.),.UNSPECIFIED.);
#149=B_SPLINE_SURFACE_WITH_KNOTS('',3,3,((#19079,#19080,#19081,#19082),
(#19083,#19084,#19085,#19086),(#19087,#19088,#19089,#19090),(#19091,#19092,
#19093,#19094),(#19095,#19096,#19097,#19098),(#19099,#19100,#19101,#19102)),
 .UNSPECIFIED.,.F.,.F.,.F.,(4,1,1,4),(4,4),(0.,0.285714285714286,0.571428571428571,
1.),(0.,1.),.UNSPECIFIED.);
#150=B_SPLINE_SURFACE_WITH_KNOTS('',3,3,((#19139,#19140,#19141,#19142),
(#19143,#19144,#19145,#19146),(#19147,#19148,#19149,#19150),(#19151,#19152,
#19153,#19154),(#19155,#19156,#19157,#19158),(#19159,#19160,#19161,#19162)),
 .UNSPECIFIED.,.F.,.F.,.F.,(4,1,1,4),(4,4),(0.,0.285714285714286,0.571428571428571,
1.),(0.,1.),.UNSPECIFIED.);
#151=B_SPLINE_SURFACE_WITH_KNOTS('',3,3,((#19199,#19200,#19201,#19202),
(#19203,#19204,#19205,#19206),(#19207,#19208,#19209,#19210),(#19211,#19212,
#19213,#19214),(#19215,#19216,#19217,#19218),(#19219,#19220,#19221,#19222)),
 .UNSPECIFIED.,.F.,.F.,.F.,(4,1,1,4),(4,4),(0.,0.285714285714286,0.571428571428571,
1.),(0.,1.),.UNSPECIFIED.);
#152=B_SPLINE_SURFACE_WITH_KNOTS('',3,3,((#19259,#19260,#19261,#19262),
(#19263,#19264,#19265,#19266),(#19267,#19268,#19269,#19270),(#19271,#19272,
#19273,#19274),(#19275,#19276,#19277,#19278),(#19279,#19280,#19281,#19282)),
 .UNSPECIFIED.,.F.,.F.,.F.,(4,1,1,4),(4,4),(0.,0.285714285714286,0.571428571428571,
1.),(0.,1.),.UNSPECIFIED.);
#153=B_SPLINE_SURFACE_WITH_KNOTS('',3,3,((#19319,#19320,#19321,#19322),
(#19323,#19324,#19325,#19326),(#19327,#19328,#19329,#19330),(#19331,#19332,
#19333,#19334),(#19335,#19336,#19337,#19338),(#19339,#19340,#19341,#19342),
(#19343,#19344,#19345,#19346),(#19347,#19348,#19349,#19350),(#19351,#19352,
#19353,#19354),(#19355,#19356,#19357,#19358),(#19359,#19360,#19361,#19362)),
 .UNSPECIFIED.,.F.,.F.,.F.,(4,1,1,1,1,1,1,1,4),(4,4),(0.,0.142857142857143,
0.285714285714286,0.357142857142857,0.428571428571429,0.571428571428571,
0.785714285714286,0.857142857142857,1.),(0.,1.),.UNSPECIFIED.);
#154=B_SPLINE_SURFACE_WITH_KNOTS('',3,3,((#19974,#19975,#19976,#19977),
(#19978,#19979,#19980,#19981),(#19982,#19983,#19984,#19985),(#19986,#19987,
#19988,#19989),(#19990,#19991,#19992,#19993),(#19994,#19995,#19996,#19997),
(#19998,#19999,#20000,#20001),(#20002,#20003,#20004,#20005),(#20006,#20007,
#20008,#20009),(#20010,#20011,#20012,#20013),(#20014,#20015,#20016,#20017)),
 .UNSPECIFIED.,.F.,.F.,.F.,(4,1,1,1,1,1,1,1,4),(4,4),(0.,0.142857142857143,
0.285714285714286,0.357142857142857,0.428571428571429,0.571428571428571,
0.785714285714286,0.857142857142857,1.),(0.,1.),.UNSPECIFIED.);
#155=B_SPLINE_SURFACE_WITH_KNOTS('',3,3,((#20025,#20026,#20027,#20028),
(#20029,#20030,#20031,#20032),(#20033,#20034,#20035,#20036),(#20037,#20038,
#20039,#20040),(#20041,#20042,#20043,#20044),(#20045,#20046,#20047,#20048),
(#20049,#20050,#20051,#20052),(#20053,#20054,#20055,#20056),(#20057,#20058,
#20059,#20060),(#20061,#20062,#20063,#20064),(#20065,#20066,#20067,#20068),
(#20069,#20070,#20071,#20072)),.UNSPECIFIED.,.F.,.F.,.F.,(4,1,1,1,1,1,1,
1,1,4),(4,4),(0.,0.142857142857143,0.285714285714286,0.321428571428571,
0.357142857142857,0.428571428571429,0.571428571428571,0.785714285714286,
0.857142857142857,1.),(0.,1.),.UNSPECIFIED.);
#156=B_SPLINE_SURFACE_WITH_KNOTS('',3,3,((#20080,#20081,#20082,#20083),
(#20084,#20085,#20086,#20087),(#20088,#20089,#20090,#20091),(#20092,#20093,
#20094,#20095),(#20096,#20097,#20098,#20099),(#20100,#20101,#20102,#20103),
(#20104,#20105,#20106,#20107),(#20108,#20109,#20110,#20111),(#20112,#20113,
#20114,#20115),(#20116,#20117,#20118,#20119),(#20120,#20121,#20122,#20123),
(#20124,#20125,#20126,#20127)),.UNSPECIFIED.,.F.,.F.,.F.,(4,1,1,1,1,1,1,
1,1,4),(4,4),(0.,0.142857142857143,0.285714285714286,0.321428571428571,
0.357142857142857,0.428571428571429,0.571428571428571,0.785714285714286,
0.857142857142857,1.),(0.,1.),.UNSPECIFIED.);
#157=B_SPLINE_SURFACE_WITH_KNOTS('',3,3,((#20135,#20136,#20137,#20138),
(#20139,#20140,#20141,#20142),(#20143,#20144,#20145,#20146),(#20147,#20148,
#20149,#20150),(#20151,#20152,#20153,#20154),(#20155,#20156,#20157,#20158),
(#20159,#20160,#20161,#20162),(#20163,#20164,#20165,#20166),(#20167,#20168,
#20169,#20170),(#20171,#20172,#20173,#20174),(#20175,#20176,#20177,#20178)),
 .UNSPECIFIED.,.F.,.F.,.F.,(4,1,1,1,1,1,1,1,4),(4,4),(0.,0.142857142857143,
0.285714285714286,0.357142857142857,0.428571428571429,0.571428571428571,
0.785714285714286,0.857142857142857,1.),(0.,1.),.UNSPECIFIED.);
#158=B_SPLINE_SURFACE_WITH_KNOTS('',3,3,((#20186,#20187,#20188,#20189),
(#20190,#20191,#20192,#20193),(#20194,#20195,#20196,#20197),(#20198,#20199,
#20200,#20201),(#20202,#20203,#20204,#20205),(#20206,#20207,#20208,#20209),
(#20210,#20211,#20212,#20213),(#20214,#20215,#20216,#20217),(#20218,#20219,
#20220,#20221),(#20222,#20223,#20224,#20225),(#20226,#20227,#20228,#20229)),
 .UNSPECIFIED.,.F.,.F.,.F.,(4,1,1,1,1,1,1,1,4),(4,4),(0.,0.142857142857143,
0.285714285714286,0.357142857142857,0.428571428571429,0.571428571428571,
0.785714285714286,0.857142857142857,1.),(0.,1.),.UNSPECIFIED.);
#159=B_SPLINE_SURFACE_WITH_KNOTS('',3,3,((#20237,#20238,#20239,#20240),
(#20241,#20242,#20243,#20244),(#20245,#20246,#20247,#20248),(#20249,#20250,
#20251,#20252),(#20253,#20254,#20255,#20256),(#20257,#20258,#20259,#20260),
(#20261,#20262,#20263,#20264),(#20265,#20266,#20267,#20268),(#20269,#20270,
#20271,#20272),(#20273,#20274,#20275,#20276),(#20277,#20278,#20279,#20280)),
 .UNSPECIFIED.,.F.,.F.,.F.,(4,1,1,1,1,1,1,1,4),(4,4),(0.,0.142857142857143,
0.285714285714286,0.357142857142857,0.428571428571429,0.571428571428571,
0.785714285714286,0.857142857142857,1.),(0.,1.),.UNSPECIFIED.);
#160=B_SPLINE_SURFACE_WITH_KNOTS('',3,3,((#20288,#20289,#20290,#20291),
(#20292,#20293,#20294,#20295),(#20296,#20297,#20298,#20299),(#20300,#20301,
#20302,#20303),(#20304,#20305,#20306,#20307),(#20308,#20309,#20310,#20311),
(#20312,#20313,#20314,#20315),(#20316,#20317,#20318,#20319),(#20320,#20321,
#20322,#20323),(#20324,#20325,#20326,#20327),(#20328,#20329,#20330,#20331),
(#20332,#20333,#20334,#20335)),.UNSPECIFIED.,.F.,.F.,.F.,(4,1,1,1,1,1,1,
1,1,4),(4,4),(0.,0.142857142857143,0.285714285714286,0.321428571428571,
0.357142857142857,0.428571428571429,0.571428571428571,0.785714285714286,
0.857142857142857,1.),(0.,1.),.UNSPECIFIED.);
#161=B_SPLINE_SURFACE_WITH_KNOTS('',3,3,((#20343,#20344,#20345,#20346),
(#20347,#20348,#20349,#20350),(#20351,#20352,#20353,#20354),(#20355,#20356,
#20357,#20358),(#20359,#20360,#20361,#20362),(#20363,#20364,#20365,#20366),
(#20367,#20368,#20369,#20370),(#20371,#20372,#20373,#20374),(#20375,#20376,
#20377,#20378),(#20379,#20380,#20381,#20382),(#20383,#20384,#20385,#20386),
(#20387,#20388,#20389,#20390)),.UNSPECIFIED.,.F.,.F.,.F.,(4,1,1,1,1,1,1,
1,1,4),(4,4),(0.,0.142857142857143,0.285714285714286,0.321428571428571,
0.357142857142857,0.428571428571429,0.571428571428571,0.785714285714286,
0.857142857142857,1.),(0.,1.),.UNSPECIFIED.);
#162=B_SPLINE_SURFACE_WITH_KNOTS('',3,3,((#20398,#20399,#20400,#20401),
(#20402,#20403,#20404,#20405),(#20406,#20407,#20408,#20409),(#20410,#20411,
#20412,#20413),(#20414,#20415,#20416,#20417),(#20418,#20419,#20420,#20421),
(#20422,#20423,#20424,#20425),(#20426,#20427,#20428,#20429),(#20430,#20431,
#20432,#20433),(#20434,#20435,#20436,#20437),(#20438,#20439,#20440,#20441)),
 .UNSPECIFIED.,.F.,.F.,.F.,(4,1,1,1,1,1,1,1,4),(4,4),(0.,0.142857142857143,
0.285714285714286,0.357142857142857,0.428571428571429,0.571428571428571,
0.785714285714286,0.857142857142857,1.),(0.,1.),.UNSPECIFIED.);
#163=B_SPLINE_SURFACE_WITH_KNOTS('',3,3,((#20449,#20450,#20451,#20452),
(#20453,#20454,#20455,#20456),(#20457,#20458,#20459,#20460),(#20461,#20462,
#20463,#20464),(#20465,#20466,#20467,#20468),(#20469,#20470,#20471,#20472),
(#20473,#20474,#20475,#20476),(#20477,#20478,#20479,#20480),(#20481,#20482,
#20483,#20484),(#20485,#20486,#20487,#20488),(#20489,#20490,#20491,#20492)),
 .UNSPECIFIED.,.F.,.F.,.F.,(4,1,1,1,1,1,1,1,4),(4,4),(0.,0.142857142857143,
0.285714285714286,0.357142857142857,0.428571428571429,0.571428571428571,
0.785714285714286,0.857142857142857,1.),(0.,1.),.UNSPECIFIED.);
#164=B_SPLINE_SURFACE_WITH_KNOTS('',3,3,((#20500,#20501,#20502,#20503),
(#20504,#20505,#20506,#20507),(#20508,#20509,#20510,#20511),(#20512,#20513,
#20514,#20515),(#20516,#20517,#20518,#20519),(#20520,#20521,#20522,#20523),
(#20524,#20525,#20526,#20527),(#20528,#20529,#20530,#20531),(#20532,#20533,
#20534,#20535),(#20536,#20537,#20538,#20539),(#20540,#20541,#20542,#20543)),
 .UNSPECIFIED.,.F.,.F.,.F.,(4,1,1,1,1,1,1,1,4),(4,4),(0.,0.142857142857143,
0.285714285714286,0.357142857142857,0.428571428571429,0.571428571428571,
0.785714285714286,0.857142857142857,1.),(0.,1.),.UNSPECIFIED.);
#165=B_SPLINE_SURFACE_WITH_KNOTS('',3,3,((#20551,#20552,#20553,#20554),
(#20555,#20556,#20557,#20558),(#20559,#20560,#20561,#20562),(#20563,#20564,
#20565,#20566),(#20567,#20568,#20569,#20570),(#20571,#20572,#20573,#20574),
(#20575,#20576,#20577,#20578),(#20579,#20580,#20581,#20582),(#20583,#20584,
#20585,#20586),(#20587,#20588,#20589,#20590),(#20591,#20592,#20593,#20594),
(#20595,#20596,#20597,#20598)),.UNSPECIFIED.,.F.,.F.,.F.,(4,1,1,1,1,1,1,
1,1,4),(4,4),(0.,0.142857142857143,0.285714285714286,0.321428571428571,
0.357142857142857,0.428571428571429,0.571428571428571,0.785714285714286,
0.857142857142857,1.),(0.,1.),.UNSPECIFIED.);
#166=B_SPLINE_SURFACE_WITH_KNOTS('',3,3,((#20606,#20607,#20608,#20609),
(#20610,#20611,#20612,#20613),(#20614,#20615,#20616,#20617),(#20618,#20619,
#20620,#20621),(#20622,#20623,#20624,#20625),(#20626,#20627,#20628,#20629),
(#20630,#20631,#20632,#20633),(#20634,#20635,#20636,#20637),(#20638,#20639,
#20640,#20641),(#20642,#20643,#20644,#20645),(#20646,#20647,#20648,#20649),
(#20650,#20651,#20652,#20653)),.UNSPECIFIED.,.F.,.F.,.F.,(4,1,1,1,1,1,1,
1,1,4),(4,4),(0.,0.142857142857143,0.285714285714286,0.321428571428571,
0.357142857142857,0.428571428571429,0.571428571428571,0.785714285714286,
0.857142857142857,1.),(0.,1.),.UNSPECIFIED.);
#167=B_SPLINE_SURFACE_WITH_KNOTS('',3,3,((#20661,#20662,#20663,#20664),
(#20665,#20666,#20667,#20668),(#20669,#20670,#20671,#20672),(#20673,#20674,
#20675,#20676),(#20677,#20678,#20679,#20680),(#20681,#20682,#20683,#20684),
(#20685,#20686,#20687,#20688),(#20689,#20690,#20691,#20692),(#20693,#20694,
#20695,#20696),(#20697,#20698,#20699,#20700),(#20701,#20702,#20703,#20704)),
 .UNSPECIFIED.,.F.,.F.,.F.,(4,1,1,1,1,1,1,1,4),(4,4),(0.,0.142857142857143,
0.285714285714286,0.357142857142857,0.428571428571429,0.571428571428571,
0.785714285714286,0.857142857142857,1.),(0.,1.),.UNSPECIFIED.);
#168=B_SPLINE_SURFACE_WITH_KNOTS('',3,3,((#20712,#20713,#20714,#20715),
(#20716,#20717,#20718,#20719),(#20720,#20721,#20722,#20723),(#20724,#20725,
#20726,#20727),(#20728,#20729,#20730,#20731),(#20732,#20733,#20734,#20735),
(#20736,#20737,#20738,#20739),(#20740,#20741,#20742,#20743),(#20744,#20745,
#20746,#20747),(#20748,#20749,#20750,#20751),(#20752,#20753,#20754,#20755)),
 .UNSPECIFIED.,.F.,.F.,.F.,(4,1,1,1,1,1,1,1,4),(4,4),(0.,0.142857142857143,
0.285714285714286,0.357142857142857,0.428571428571429,0.571428571428571,
0.785714285714286,0.857142857142857,1.),(0.,1.),.UNSPECIFIED.);
#169=B_SPLINE_SURFACE_WITH_KNOTS('',3,3,((#20763,#20764,#20765,#20766),
(#20767,#20768,#20769,#20770),(#20771,#20772,#20773,#20774),(#20775,#20776,
#20777,#20778),(#20779,#20780,#20781,#20782),(#20783,#20784,#20785,#20786),
(#20787,#20788,#20789,#20790),(#20791,#20792,#20793,#20794),(#20795,#20796,
#20797,#20798),(#20799,#20800,#20801,#20802),(#20803,#20804,#20805,#20806)),
 .UNSPECIFIED.,.F.,.F.,.F.,(4,1,1,1,1,1,1,1,4),(4,4),(0.,0.142857142857143,
0.285714285714286,0.357142857142857,0.428571428571429,0.571428571428571,
0.785714285714286,0.857142857142857,1.),(0.,1.),.UNSPECIFIED.);
#170=B_SPLINE_SURFACE_WITH_KNOTS('',3,3,((#20814,#20815,#20816,#20817),
(#20818,#20819,#20820,#20821),(#20822,#20823,#20824,#20825),(#20826,#20827,
#20828,#20829),(#20830,#20831,#20832,#20833),(#20834,#20835,#20836,#20837),
(#20838,#20839,#20840,#20841),(#20842,#20843,#20844,#20845),(#20846,#20847,
#20848,#20849),(#20850,#20851,#20852,#20853),(#20854,#20855,#20856,#20857),
(#20858,#20859,#20860,#20861)),.UNSPECIFIED.,.F.,.F.,.F.,(4,1,1,1,1,1,1,
1,1,4),(4,4),(0.,0.142857142857143,0.285714285714286,0.321428571428571,
0.357142857142857,0.428571428571429,0.571428571428571,0.785714285714286,
0.857142857142857,1.),(0.,1.),.UNSPECIFIED.);
#171=B_SPLINE_SURFACE_WITH_KNOTS('',3,3,((#20869,#20870,#20871,#20872),
(#20873,#20874,#20875,#20876),(#20877,#20878,#20879,#20880),(#20881,#20882,
#20883,#20884),(#20885,#20886,#20887,#20888),(#20889,#20890,#20891,#20892),
(#20893,#20894,#20895,#20896),(#20897,#20898,#20899,#20900),(#20901,#20902,
#20903,#20904),(#20905,#20906,#20907,#20908),(#20909,#20910,#20911,#20912),
(#20913,#20914,#20915,#20916)),.UNSPECIFIED.,.F.,.F.,.F.,(4,1,1,1,1,1,1,
1,1,4),(4,4),(0.,0.142857142857143,0.285714285714286,0.321428571428571,
0.357142857142857,0.428571428571429,0.571428571428571,0.785714285714286,
0.857142857142857,1.),(0.,1.),.UNSPECIFIED.);
#172=B_SPLINE_SURFACE_WITH_KNOTS('',3,3,((#20924,#20925,#20926,#20927),
(#20928,#20929,#20930,#20931),(#20932,#20933,#20934,#20935),(#20936,#20937,
#20938,#20939),(#20940,#20941,#20942,#20943),(#20944,#20945,#20946,#20947),
(#20948,#20949,#20950,#20951),(#20952,#20953,#20954,#20955),(#20956,#20957,
#20958,#20959),(#20960,#20961,#20962,#20963),(#20964,#20965,#20966,#20967)),
 .UNSPECIFIED.,.F.,.F.,.F.,(4,1,1,1,1,1,1,1,4),(4,4),(0.,0.142857142857143,
0.285714285714286,0.357142857142857,0.428571428571429,0.571428571428571,
0.785714285714286,0.857142857142857,1.),(0.,1.),.UNSPECIFIED.);
#173=B_SPLINE_SURFACE_WITH_KNOTS('',3,3,((#22595,#22596,#22597,#22598,#22599,
#22600,#22601,#22602,#22603,#22604,#22605,#22606,#22607,#22608,#22609,#22610,
#22611,#22612,#22613,#22614,#22615,#22616,#22617,#22618,#22619,#22620,#22621,
#22622,#22623,#22624,#22625,#22626,#22627,#22628,#22629),(#22630,#22631,
#22632,#22633,#22634,#22635,#22636,#22637,#22638,#22639,#22640,#22641,#22642,
#22643,#22644,#22645,#22646,#22647,#22648,#22649,#22650,#22651,#22652,#22653,
#22654,#22655,#22656,#22657,#22658,#22659,#22660,#22661,#22662,#22663,#22664),
(#22665,#22666,#22667,#22668,#22669,#22670,#22671,#22672,#22673,#22674,
#22675,#22676,#22677,#22678,#22679,#22680,#22681,#22682,#22683,#22684,#22685,
#22686,#22687,#22688,#22689,#22690,#22691,#22692,#22693,#22694,#22695,#22696,
#22697,#22698,#22699),(#22700,#22701,#22702,#22703,#22704,#22705,#22706,
#22707,#22708,#22709,#22710,#22711,#22712,#22713,#22714,#22715,#22716,#22717,
#22718,#22719,#22720,#22721,#22722,#22723,#22724,#22725,#22726,#22727,#22728,
#22729,#22730,#22731,#22732,#22733,#22734)),.UNSPECIFIED.,.F.,.F.,.F.,(4,
4),(4,1,1,1,1,1,1,1,1,1,1,1,1,1,1,1,1,1,1,1,1,1,1,1,1,1,1,1,1,1,1,1,4),
(0.,0.0460148164544132),(8.31058692273979,9.28321112839862,10.2558353340575,
11.2284595397163,12.2010837453751,13.173707951034,14.1463321566928,15.1189563623516,
16.0915805680104,17.0642047736693,18.0368289793281,19.0094531849869,19.9820773906458,
20.9547015963046,21.9273258019634,22.8999500076223,23.8725742132811,24.8451984189399,
25.8178226245988,26.7904468302576,27.7630710359164,28.7356952415753,29.7083194472341,
30.6809436528929,31.6535678585518,32.6261920642106,33.5988162698694,34.5714404755283,
35.5440646811871,36.5166888868459,37.4893130925048,38.4619372981636,39.4345615038224),
 .UNSPECIFIED.);
#174=B_SPLINE_SURFACE_WITH_KNOTS('',3,3,((#22949,#22950,#22951,#22952,#22953,
#22954,#22955,#22956,#22957,#22958,#22959,#22960,#22961,#22962,#22963,#22964,
#22965,#22966,#22967,#22968,#22969,#22970,#22971,#22972,#22973,#22974,#22975,
#22976,#22977,#22978,#22979,#22980,#22981,#22982,#22983),(#22984,#22985,
#22986,#22987,#22988,#22989,#22990,#22991,#22992,#22993,#22994,#22995,#22996,
#22997,#22998,#22999,#23000,#23001,#23002,#23003,#23004,#23005,#23006,#23007,
#23008,#23009,#23010,#23011,#23012,#23013,#23014,#23015,#23016,#23017,#23018),
(#23019,#23020,#23021,#23022,#23023,#23024,#23025,#23026,#23027,#23028,
#23029,#23030,#23031,#23032,#23033,#23034,#23035,#23036,#23037,#23038,#23039,
#23040,#23041,#23042,#23043,#23044,#23045,#23046,#23047,#23048,#23049,#23050,
#23051,#23052,#23053),(#23054,#23055,#23056,#23057,#23058,#23059,#23060,
#23061,#23062,#23063,#23064,#23065,#23066,#23067,#23068,#23069,#23070,#23071,
#23072,#23073,#23074,#23075,#23076,#23077,#23078,#23079,#23080,#23081,#23082,
#23083,#23084,#23085,#23086,#23087,#23088)),.UNSPECIFIED.,.F.,.F.,.F.,(4,
4),(4,1,1,1,1,1,1,1,1,1,1,1,1,1,1,1,1,1,1,1,1,1,1,1,1,1,1,1,1,1,1,1,4),
(0.,0.0460148164544132),(11.6154215191107,12.5880457247695,13.5606699304283,
14.5332941360872,15.505918341746,16.4785425474048,17.4511667530637,18.4237909587225,
19.3964151643813,20.3690393700402,21.341663575699,22.3142877813578,23.2869119870167,
24.2595361926755,25.2321603983343,26.2047846039932,27.177408809652,28.1500330153108,
29.1226572209696,30.0952814266285,31.0679056322873,32.0405298379462,33.013154043605,
33.9857782492638,34.9584024549226,35.9310266605815,36.9036508662403,37.8762750718991,
38.848899277558,39.8215234832168,40.7941476888756,41.7667718945345,42.7393961001933),
 .UNSPECIFIED.);
#175=(
BOUNDED_CURVE()
B_SPLINE_CURVE(5,(#9974,#9975,#9976,#9977,#9978,#9979,#9980,#9981,#9982,
#9983,#9984,#9985,#9986,#9987,#9988,#9989,#9990,#9991,#9992,#9993,#9994,
#9995,#9996,#9997,#9998,#9999,#10000,#10001,#10002,#10003,#10004,#10005,
#10006,#10007,#10008),.UNSPECIFIED.,.F.,.F.)
B_SPLINE_CURVE_WITH_KNOTS((6,1,1,1,1,1,1,1,1,1,1,1,1,1,1,1,1,1,1,1,1,1,
1,1,1,1,1,1,1,1,6),(0.,0.0333333333333333,0.0666666666666667,0.1,0.133333333333333,
0.166666666666667,0.2,0.233333333333333,0.266666666666667,0.3,0.333333333333333,
0.366666666666667,0.4,0.433333333333333,0.466666666666667,0.5,0.533333333333333,
0.566666666666667,0.6,0.633333333333333,0.666666666666667,0.7,0.733333333333333,
0.766666666666667,0.8,0.833333333333333,0.866666666666667,0.9,0.933333333333333,
0.966666666666667,1.),.UNSPECIFIED.)
CURVE()
GEOMETRIC_REPRESENTATION_ITEM()
RATIONAL_B_SPLINE_CURVE((1.,1.,1.,1.,1.,1.,1.,1.,1.,1.,1.,1.,1.,1.,1.,1.,
1.,1.,1.,1.,1.,1.,1.,1.,1.,1.,1.,1.,1.,1.,1.,1.,1.,1.,1.))
REPRESENTATION_ITEM('')
);
#176=(
BOUNDED_CURVE()
B_SPLINE_CURVE(5,(#10010,#10011,#10012,#10013,#10014,#10015,#10016,#10017,
#10018,#10019,#10020,#10021,#10022,#10023,#10024,#10025,#10026,#10027,#10028,
#10029,#10030,#10031,#10032,#10033,#10034,#10035,#10036,#10037,#10038,#10039,
#10040,#10041,#10042,#10043,#10044),.UNSPECIFIED.,.F.,.F.)
B_SPLINE_CURVE_WITH_KNOTS((6,1,1,1,1,1,1,1,1,1,1,1,1,1,1,1,1,1,1,1,1,1,
1,1,1,1,1,1,1,1,6),(0.,0.0333333333333333,0.0666666666666667,0.1,0.133333333333333,
0.166666666666667,0.2,0.233333333333333,0.266666666666667,0.3,0.333333333333333,
0.366666666666667,0.4,0.433333333333333,0.466666666666667,0.5,0.533333333333333,
0.566666666666667,0.6,0.633333333333333,0.666666666666667,0.7,0.733333333333333,
0.766666666666667,0.8,0.833333333333333,0.866666666666667,0.9,0.933333333333333,
0.966666666666667,1.),.UNSPECIFIED.)
CURVE()
GEOMETRIC_REPRESENTATION_ITEM()
RATIONAL_B_SPLINE_CURVE((1.,1.,1.,1.,1.,1.,1.,1.,1.,1.,1.,1.,1.,1.,1.,1.,
1.,1.,1.,1.,1.,1.,1.,1.,1.,1.,1.,1.,1.,1.,1.,1.,1.,1.,1.))
REPRESENTATION_ITEM('')
);
#177=(
BOUNDED_CURVE()
B_SPLINE_CURVE(5,(#10048,#10049,#10050,#10051,#10052,#10053,#10054,#10055,
#10056,#10057,#10058,#10059,#10060,#10061,#10062,#10063,#10064,#10065,#10066,
#10067,#10068,#10069,#10070,#10071,#10072,#10073,#10074,#10075,#10076,#10077,
#10078,#10079,#10080,#10081,#10082),.UNSPECIFIED.,.F.,.F.)
B_SPLINE_CURVE_WITH_KNOTS((6,1,1,1,1,1,1,1,1,1,1,1,1,1,1,1,1,1,1,1,1,1,
1,1,1,1,1,1,1,1,6),(0.,0.0333333333333333,0.0666666666666667,0.1,0.133333333333333,
0.166666666666667,0.2,0.233333333333333,0.266666666666667,0.3,0.333333333333333,
0.366666666666667,0.4,0.433333333333333,0.466666666666667,0.5,0.533333333333333,
0.566666666666667,0.6,0.633333333333333,0.666666666666667,0.7,0.733333333333333,
0.766666666666667,0.8,0.833333333333333,0.866666666666667,0.9,0.933333333333333,
0.966666666666667,1.),.UNSPECIFIED.)
CURVE()
GEOMETRIC_REPRESENTATION_ITEM()
RATIONAL_B_SPLINE_CURVE((1.,1.,1.,1.,1.,1.,1.,1.,1.,1.,1.,1.,1.,1.,1.,1.,
1.,1.,1.,1.,1.,1.,1.,1.,1.,1.,1.,1.,1.,1.,1.,1.,1.,1.,1.))
REPRESENTATION_ITEM('')
);
#178=(
BOUNDED_CURVE()
B_SPLINE_CURVE(5,(#10084,#10085,#10086,#10087,#10088,#10089,#10090,#10091,
#10092,#10093,#10094,#10095,#10096,#10097,#10098,#10099,#10100,#10101,#10102,
#10103,#10104,#10105,#10106,#10107,#10108,#10109,#10110,#10111,#10112,#10113,
#10114,#10115,#10116,#10117,#10118),.UNSPECIFIED.,.F.,.F.)
B_SPLINE_CURVE_WITH_KNOTS((6,1,1,1,1,1,1,1,1,1,1,1,1,1,1,1,1,1,1,1,1,1,
1,1,1,1,1,1,1,1,6),(0.,0.0333333333333333,0.0666666666666667,0.1,0.133333333333333,
0.166666666666667,0.2,0.233333333333333,0.266666666666667,0.3,0.333333333333333,
0.366666666666667,0.4,0.433333333333333,0.466666666666667,0.5,0.533333333333333,
0.566666666666667,0.6,0.633333333333333,0.666666666666667,0.7,0.733333333333333,
0.766666666666667,0.8,0.833333333333333,0.866666666666667,0.9,0.933333333333333,
0.966666666666667,1.),.UNSPECIFIED.)
CURVE()
GEOMETRIC_REPRESENTATION_ITEM()
RATIONAL_B_SPLINE_CURVE((1.,1.,1.,1.,1.,1.,1.,1.,1.,1.,1.,1.,1.,1.,1.,1.,
1.,1.,1.,1.,1.,1.,1.,1.,1.,1.,1.,1.,1.,1.,1.,1.,1.,1.,1.))
REPRESENTATION_ITEM('')
);
#179=(
BOUNDED_CURVE()
B_SPLINE_CURVE(5,(#10122,#10123,#10124,#10125,#10126,#10127,#10128,#10129,
#10130,#10131,#10132,#10133,#10134,#10135,#10136,#10137,#10138,#10139,#10140,
#10141,#10142,#10143,#10144,#10145,#10146,#10147,#10148,#10149,#10150,#10151,
#10152,#10153,#10154,#10155,#10156),.UNSPECIFIED.,.F.,.F.)
B_SPLINE_CURVE_WITH_KNOTS((6,1,1,1,1,1,1,1,1,1,1,1,1,1,1,1,1,1,1,1,1,1,
1,1,1,1,1,1,1,1,6),(0.,0.0333333333333333,0.0666666666666667,0.1,0.133333333333333,
0.166666666666667,0.2,0.233333333333333,0.266666666666667,0.3,0.333333333333333,
0.366666666666667,0.4,0.433333333333333,0.466666666666667,0.5,0.533333333333333,
0.566666666666667,0.6,0.633333333333333,0.666666666666667,0.7,0.733333333333333,
0.766666666666667,0.8,0.833333333333333,0.866666666666667,0.9,0.933333333333333,
0.966666666666667,1.),.UNSPECIFIED.)
CURVE()
GEOMETRIC_REPRESENTATION_ITEM()
RATIONAL_B_SPLINE_CURVE((1.,1.,1.,1.,1.,1.,1.,1.,1.,1.,1.,1.,1.,1.,1.,1.,
1.,1.,1.,1.,1.,1.,1.,1.,1.,1.,1.,1.,1.,1.,1.,1.,1.,1.,1.))
REPRESENTATION_ITEM('')
);
#180=(
BOUNDED_CURVE()
B_SPLINE_CURVE(5,(#10158,#10159,#10160,#10161,#10162,#10163,#10164,#10165,
#10166,#10167,#10168,#10169,#10170,#10171,#10172,#10173,#10174,#10175,#10176,
#10177,#10178,#10179,#10180,#10181,#10182,#10183,#10184,#10185,#10186,#10187,
#10188,#10189,#10190,#10191,#10192),.UNSPECIFIED.,.F.,.F.)
B_SPLINE_CURVE_WITH_KNOTS((6,1,1,1,1,1,1,1,1,1,1,1,1,1,1,1,1,1,1,1,1,1,
1,1,1,1,1,1,1,1,6),(0.,0.0333333333333333,0.0666666666666667,0.1,0.133333333333333,
0.166666666666667,0.2,0.233333333333333,0.266666666666667,0.3,0.333333333333333,
0.366666666666667,0.4,0.433333333333333,0.466666666666667,0.5,0.533333333333333,
0.566666666666667,0.6,0.633333333333333,0.666666666666667,0.7,0.733333333333333,
0.766666666666667,0.8,0.833333333333333,0.866666666666667,0.9,0.933333333333333,
0.966666666666667,1.),.UNSPECIFIED.)
CURVE()
GEOMETRIC_REPRESENTATION_ITEM()
RATIONAL_B_SPLINE_CURVE((1.,1.,1.,1.,1.,1.,1.,1.,1.,1.,1.,1.,1.,1.,1.,1.,
1.,1.,1.,1.,1.,1.,1.,1.,1.,1.,1.,1.,1.,1.,1.,1.,1.,1.,1.))
REPRESENTATION_ITEM('')
);
#181=(
BOUNDED_CURVE()
B_SPLINE_CURVE(5,(#10196,#10197,#10198,#10199,#10200,#10201,#10202,#10203,
#10204,#10205,#10206,#10207,#10208,#10209,#10210,#10211,#10212,#10213,#10214,
#10215,#10216,#10217,#10218,#10219,#10220,#10221,#10222,#10223,#10224,#10225,
#10226,#10227,#10228,#10229,#10230),.UNSPECIFIED.,.F.,.F.)
B_SPLINE_CURVE_WITH_KNOTS((6,1,1,1,1,1,1,1,1,1,1,1,1,1,1,1,1,1,1,1,1,1,
1,1,1,1,1,1,1,1,6),(0.,0.0333333333333333,0.0666666666666667,0.1,0.133333333333333,
0.166666666666667,0.2,0.233333333333333,0.266666666666667,0.3,0.333333333333333,
0.366666666666667,0.4,0.433333333333333,0.466666666666667,0.5,0.533333333333333,
0.566666666666667,0.6,0.633333333333333,0.666666666666667,0.7,0.733333333333333,
0.766666666666667,0.8,0.833333333333333,0.866666666666667,0.9,0.933333333333333,
0.966666666666667,1.),.UNSPECIFIED.)
CURVE()
GEOMETRIC_REPRESENTATION_ITEM()
RATIONAL_B_SPLINE_CURVE((1.,1.,1.,1.,1.,1.,1.,1.,1.,1.,1.,1.,1.,1.,1.,1.,
1.,1.,1.,1.,1.,1.,1.,1.,1.,1.,1.,1.,1.,1.,1.,1.,1.,1.,1.))
REPRESENTATION_ITEM('')
);
#182=(
BOUNDED_CURVE()
B_SPLINE_CURVE(5,(#10232,#10233,#10234,#10235,#10236,#10237,#10238,#10239,
#10240,#10241,#10242,#10243,#10244,#10245,#10246,#10247,#10248,#10249,#10250,
#10251,#10252,#10253,#10254,#10255,#10256,#10257,#10258,#10259,#10260,#10261,
#10262,#10263,#10264,#10265,#10266),.UNSPECIFIED.,.F.,.F.)
B_SPLINE_CURVE_WITH_KNOTS((6,1,1,1,1,1,1,1,1,1,1,1,1,1,1,1,1,1,1,1,1,1,
1,1,1,1,1,1,1,1,6),(0.,0.0333333333333333,0.0666666666666667,0.1,0.133333333333333,
0.166666666666667,0.2,0.233333333333333,0.266666666666667,0.3,0.333333333333333,
0.366666666666667,0.4,0.433333333333333,0.466666666666667,0.5,0.533333333333333,
0.566666666666667,0.6,0.633333333333333,0.666666666666667,0.7,0.733333333333333,
0.766666666666667,0.8,0.833333333333333,0.866666666666667,0.9,0.933333333333333,
0.966666666666667,1.),.UNSPECIFIED.)
CURVE()
GEOMETRIC_REPRESENTATION_ITEM()
RATIONAL_B_SPLINE_CURVE((1.,1.,1.,1.,1.,1.,1.,1.,1.,1.,1.,1.,1.,1.,1.,1.,
1.,1.,1.,1.,1.,1.,1.,1.,1.,1.,1.,1.,1.,1.,1.,1.,1.,1.,1.))
REPRESENTATION_ITEM('')
);
#183=(
BOUNDED_CURVE()
B_SPLINE_CURVE(5,(#10270,#10271,#10272,#10273,#10274,#10275,#10276,#10277,
#10278,#10279,#10280,#10281,#10282,#10283,#10284,#10285,#10286,#10287,#10288,
#10289,#10290,#10291,#10292,#10293,#10294,#10295,#10296,#10297,#10298,#10299,
#10300,#10301,#10302,#10303,#10304),.UNSPECIFIED.,.F.,.F.)
B_SPLINE_CURVE_WITH_KNOTS((6,1,1,1,1,1,1,1,1,1,1,1,1,1,1,1,1,1,1,1,1,1,
1,1,1,1,1,1,1,1,6),(0.,0.0333333333333333,0.0666666666666667,0.1,0.133333333333333,
0.166666666666667,0.2,0.233333333333333,0.266666666666667,0.3,0.333333333333333,
0.366666666666667,0.4,0.433333333333333,0.466666666666667,0.5,0.533333333333333,
0.566666666666667,0.6,0.633333333333333,0.666666666666667,0.7,0.733333333333333,
0.766666666666667,0.8,0.833333333333333,0.866666666666667,0.9,0.933333333333333,
0.966666666666667,1.),.UNSPECIFIED.)
CURVE()
GEOMETRIC_REPRESENTATION_ITEM()
RATIONAL_B_SPLINE_CURVE((1.,1.,1.,1.,1.,1.,1.,1.,1.,1.,1.,1.,1.,1.,1.,1.,
1.,1.,1.,1.,1.,1.,1.,1.,1.,1.,1.,1.,1.,1.,1.,1.,1.,1.,1.))
REPRESENTATION_ITEM('')
);
#184=(
BOUNDED_CURVE()
B_SPLINE_CURVE(5,(#10306,#10307,#10308,#10309,#10310,#10311,#10312,#10313,
#10314,#10315,#10316,#10317,#10318,#10319,#10320,#10321,#10322,#10323,#10324,
#10325,#10326,#10327,#10328,#10329,#10330,#10331,#10332,#10333,#10334,#10335,
#10336,#10337,#10338,#10339,#10340),.UNSPECIFIED.,.F.,.F.)
B_SPLINE_CURVE_WITH_KNOTS((6,1,1,1,1,1,1,1,1,1,1,1,1,1,1,1,1,1,1,1,1,1,
1,1,1,1,1,1,1,1,6),(0.,0.0333333333333333,0.0666666666666667,0.1,0.133333333333333,
0.166666666666667,0.2,0.233333333333333,0.266666666666667,0.3,0.333333333333333,
0.366666666666667,0.4,0.433333333333333,0.466666666666667,0.5,0.533333333333333,
0.566666666666667,0.6,0.633333333333333,0.666666666666667,0.7,0.733333333333333,
0.766666666666667,0.8,0.833333333333333,0.866666666666667,0.9,0.933333333333333,
0.966666666666667,1.),.UNSPECIFIED.)
CURVE()
GEOMETRIC_REPRESENTATION_ITEM()
RATIONAL_B_SPLINE_CURVE((1.,1.,1.,1.,1.,1.,1.,1.,1.,1.,1.,1.,1.,1.,1.,1.,
1.,1.,1.,1.,1.,1.,1.,1.,1.,1.,1.,1.,1.,1.,1.,1.,1.,1.,1.))
REPRESENTATION_ITEM('')
);
#185=(
BOUNDED_CURVE()
B_SPLINE_CURVE(5,(#10344,#10345,#10346,#10347,#10348,#10349,#10350,#10351,
#10352,#10353,#10354,#10355,#10356,#10357,#10358,#10359,#10360,#10361,#10362,
#10363,#10364,#10365,#10366,#10367,#10368,#10369,#10370,#10371,#10372,#10373,
#10374,#10375,#10376,#10377,#10378),.UNSPECIFIED.,.F.,.F.)
B_SPLINE_CURVE_WITH_KNOTS((6,1,1,1,1,1,1,1,1,1,1,1,1,1,1,1,1,1,1,1,1,1,
1,1,1,1,1,1,1,1,6),(0.,0.0333333333333333,0.0666666666666667,0.1,0.133333333333333,
0.166666666666667,0.2,0.233333333333333,0.266666666666667,0.3,0.333333333333333,
0.366666666666667,0.4,0.433333333333333,0.466666666666667,0.5,0.533333333333333,
0.566666666666667,0.6,0.633333333333333,0.666666666666667,0.7,0.733333333333333,
0.766666666666667,0.8,0.833333333333333,0.866666666666667,0.9,0.933333333333333,
0.966666666666667,1.),.UNSPECIFIED.)
CURVE()
GEOMETRIC_REPRESENTATION_ITEM()
RATIONAL_B_SPLINE_CURVE((1.,1.,1.,1.,1.,1.,1.,1.,1.,1.,1.,1.,1.,1.,1.,1.,
1.,1.,1.,1.,1.,1.,1.,1.,1.,1.,1.,1.,1.,1.,1.,1.,1.,1.,1.))
REPRESENTATION_ITEM('')
);
#186=(
BOUNDED_CURVE()
B_SPLINE_CURVE(5,(#10380,#10381,#10382,#10383,#10384,#10385,#10386,#10387,
#10388,#10389,#10390,#10391,#10392,#10393,#10394,#10395,#10396,#10397,#10398,
#10399,#10400,#10401,#10402,#10403,#10404,#10405,#10406,#10407,#10408,#10409,
#10410,#10411,#10412,#10413,#10414),.UNSPECIFIED.,.F.,.F.)
B_SPLINE_CURVE_WITH_KNOTS((6,1,1,1,1,1,1,1,1,1,1,1,1,1,1,1,1,1,1,1,1,1,
1,1,1,1,1,1,1,1,6),(0.,0.0333333333333333,0.0666666666666667,0.1,0.133333333333333,
0.166666666666667,0.2,0.233333333333333,0.266666666666667,0.3,0.333333333333333,
0.366666666666667,0.4,0.433333333333333,0.466666666666667,0.5,0.533333333333333,
0.566666666666667,0.6,0.633333333333333,0.666666666666667,0.7,0.733333333333333,
0.766666666666667,0.8,0.833333333333333,0.866666666666667,0.9,0.933333333333333,
0.966666666666667,1.),.UNSPECIFIED.)
CURVE()
GEOMETRIC_REPRESENTATION_ITEM()
RATIONAL_B_SPLINE_CURVE((1.,1.,1.,1.,1.,1.,1.,1.,1.,1.,1.,1.,1.,1.,1.,1.,
1.,1.,1.,1.,1.,1.,1.,1.,1.,1.,1.,1.,1.,1.,1.,1.,1.,1.,1.))
REPRESENTATION_ITEM('')
);
#187=(
BOUNDED_CURVE()
B_SPLINE_CURVE(5,(#10418,#10419,#10420,#10421,#10422,#10423,#10424,#10425,
#10426,#10427,#10428,#10429,#10430,#10431,#10432,#10433,#10434,#10435,#10436,
#10437,#10438,#10439,#10440,#10441,#10442,#10443,#10444,#10445,#10446,#10447,
#10448,#10449,#10450,#10451,#10452),.UNSPECIFIED.,.F.,.F.)
B_SPLINE_CURVE_WITH_KNOTS((6,1,1,1,1,1,1,1,1,1,1,1,1,1,1,1,1,1,1,1,1,1,
1,1,1,1,1,1,1,1,6),(0.,0.0333333333333333,0.0666666666666667,0.1,0.133333333333333,
0.166666666666667,0.2,0.233333333333333,0.266666666666667,0.3,0.333333333333333,
0.366666666666667,0.4,0.433333333333333,0.466666666666667,0.5,0.533333333333333,
0.566666666666667,0.6,0.633333333333333,0.666666666666667,0.7,0.733333333333333,
0.766666666666667,0.8,0.833333333333333,0.866666666666667,0.9,0.933333333333333,
0.966666666666667,1.),.UNSPECIFIED.)
CURVE()
GEOMETRIC_REPRESENTATION_ITEM()
RATIONAL_B_SPLINE_CURVE((1.,1.,1.,1.,1.,1.,1.,1.,1.,1.,1.,1.,1.,1.,1.,1.,
1.,1.,1.,1.,1.,1.,1.,1.,1.,1.,1.,1.,1.,1.,1.,1.,1.,1.,1.))
REPRESENTATION_ITEM('')
);
#188=(
BOUNDED_CURVE()
B_SPLINE_CURVE(5,(#10454,#10455,#10456,#10457,#10458,#10459,#10460,#10461,
#10462,#10463,#10464,#10465,#10466,#10467,#10468,#10469,#10470,#10471,#10472,
#10473,#10474,#10475,#10476,#10477,#10478,#10479,#10480,#10481,#10482,#10483,
#10484,#10485,#10486,#10487,#10488),.UNSPECIFIED.,.F.,.F.)
B_SPLINE_CURVE_WITH_KNOTS((6,1,1,1,1,1,1,1,1,1,1,1,1,1,1,1,1,1,1,1,1,1,
1,1,1,1,1,1,1,1,6),(0.,0.0333333333333333,0.0666666666666667,0.1,0.133333333333333,
0.166666666666667,0.2,0.233333333333333,0.266666666666667,0.3,0.333333333333333,
0.366666666666667,0.4,0.433333333333333,0.466666666666667,0.5,0.533333333333333,
0.566666666666667,0.6,0.633333333333333,0.666666666666667,0.7,0.733333333333333,
0.766666666666667,0.8,0.833333333333333,0.866666666666667,0.9,0.933333333333333,
0.966666666666667,1.),.UNSPECIFIED.)
CURVE()
GEOMETRIC_REPRESENTATION_ITEM()
RATIONAL_B_SPLINE_CURVE((1.,1.,1.,1.,1.,1.,1.,1.,1.,1.,1.,1.,1.,1.,1.,1.,
1.,1.,1.,1.,1.,1.,1.,1.,1.,1.,1.,1.,1.,1.,1.,1.,1.,1.,1.))
REPRESENTATION_ITEM('')
);
#189=(
BOUNDED_CURVE()
B_SPLINE_CURVE(5,(#10492,#10493,#10494,#10495,#10496,#10497,#10498,#10499,
#10500,#10501,#10502,#10503,#10504,#10505,#10506,#10507,#10508,#10509,#10510,
#10511,#10512,#10513,#10514,#10515,#10516,#10517,#10518,#10519,#10520,#10521,
#10522,#10523,#10524,#10525,#10526),.UNSPECIFIED.,.F.,.F.)
B_SPLINE_CURVE_WITH_KNOTS((6,1,1,1,1,1,1,1,1,1,1,1,1,1,1,1,1,1,1,1,1,1,
1,1,1,1,1,1,1,1,6),(0.,0.0333333333333333,0.0666666666666667,0.1,0.133333333333333,
0.166666666666667,0.2,0.233333333333333,0.266666666666667,0.3,0.333333333333333,
0.366666666666667,0.4,0.433333333333333,0.466666666666667,0.5,0.533333333333333,
0.566666666666667,0.6,0.633333333333333,0.666666666666667,0.7,0.733333333333333,
0.766666666666667,0.8,0.833333333333333,0.866666666666667,0.9,0.933333333333333,
0.966666666666667,1.),.UNSPECIFIED.)
CURVE()
GEOMETRIC_REPRESENTATION_ITEM()
RATIONAL_B_SPLINE_CURVE((1.,1.,1.,1.,1.,1.,1.,1.,1.,1.,1.,1.,1.,1.,1.,1.,
1.,1.,1.,1.,1.,1.,1.,1.,1.,1.,1.,1.,1.,1.,1.,1.,1.,1.,1.))
REPRESENTATION_ITEM('')
);
#190=(
BOUNDED_CURVE()
B_SPLINE_CURVE(5,(#10528,#10529,#10530,#10531,#10532,#10533,#10534,#10535,
#10536,#10537,#10538,#10539,#10540,#10541,#10542,#10543,#10544,#10545,#10546,
#10547,#10548,#10549,#10550,#10551,#10552,#10553,#10554,#10555,#10556,#10557,
#10558,#10559,#10560,#10561,#10562),.UNSPECIFIED.,.F.,.F.)
B_SPLINE_CURVE_WITH_KNOTS((6,1,1,1,1,1,1,1,1,1,1,1,1,1,1,1,1,1,1,1,1,1,
1,1,1,1,1,1,1,1,6),(0.,0.0333333333333333,0.0666666666666667,0.1,0.133333333333333,
0.166666666666667,0.2,0.233333333333333,0.266666666666667,0.3,0.333333333333333,
0.366666666666667,0.4,0.433333333333333,0.466666666666667,0.5,0.533333333333333,
0.566666666666667,0.6,0.633333333333333,0.666666666666667,0.7,0.733333333333333,
0.766666666666667,0.8,0.833333333333333,0.866666666666667,0.9,0.933333333333333,
0.966666666666667,1.),.UNSPECIFIED.)
CURVE()
GEOMETRIC_REPRESENTATION_ITEM()
RATIONAL_B_SPLINE_CURVE((1.,1.,1.,1.,1.,1.,1.,1.,1.,1.,1.,1.,1.,1.,1.,1.,
1.,1.,1.,1.,1.,1.,1.,1.,1.,1.,1.,1.,1.,1.,1.,1.,1.,1.,1.))
REPRESENTATION_ITEM('')
);
#191=(
BOUNDED_CURVE()
B_SPLINE_CURVE(5,(#10566,#10567,#10568,#10569,#10570,#10571,#10572,#10573,
#10574,#10575,#10576,#10577,#10578,#10579,#10580,#10581,#10582,#10583,#10584,
#10585,#10586,#10587,#10588,#10589,#10590,#10591,#10592,#10593,#10594,#10595,
#10596,#10597,#10598,#10599,#10600),.UNSPECIFIED.,.F.,.F.)
B_SPLINE_CURVE_WITH_KNOTS((6,1,1,1,1,1,1,1,1,1,1,1,1,1,1,1,1,1,1,1,1,1,
1,1,1,1,1,1,1,1,6),(0.,0.0333333333333333,0.0666666666666667,0.1,0.133333333333333,
0.166666666666667,0.2,0.233333333333333,0.266666666666667,0.3,0.333333333333333,
0.366666666666667,0.4,0.433333333333333,0.466666666666667,0.5,0.533333333333333,
0.566666666666667,0.6,0.633333333333333,0.666666666666667,0.7,0.733333333333333,
0.766666666666667,0.8,0.833333333333333,0.866666666666667,0.9,0.933333333333333,
0.966666666666667,1.),.UNSPECIFIED.)
CURVE()
GEOMETRIC_REPRESENTATION_ITEM()
RATIONAL_B_SPLINE_CURVE((1.,1.,1.,1.,1.,1.,1.,1.,1.,1.,1.,1.,1.,1.,1.,1.,
1.,1.,1.,1.,1.,1.,1.,1.,1.,1.,1.,1.,1.,1.,1.,1.,1.,1.,1.))
REPRESENTATION_ITEM('')
);
#192=(
BOUNDED_CURVE()
B_SPLINE_CURVE(5,(#10601,#10602,#10603,#10604,#10605,#10606,#10607,#10608,
#10609,#10610,#10611,#10612,#10613,#10614,#10615,#10616,#10617,#10618,#10619,
#10620,#10621,#10622,#10623,#10624,#10625,#10626,#10627,#10628,#10629,#10630,
#10631,#10632,#10633,#10634,#10635),.UNSPECIFIED.,.F.,.F.)
B_SPLINE_CURVE_WITH_KNOTS((6,1,1,1,1,1,1,1,1,1,1,1,1,1,1,1,1,1,1,1,1,1,
1,1,1,1,1,1,1,1,6),(0.,0.0333333333333333,0.0666666666666667,0.1,0.133333333333333,
0.166666666666667,0.2,0.233333333333333,0.266666666666667,0.3,0.333333333333333,
0.366666666666667,0.4,0.433333333333333,0.466666666666667,0.5,0.533333333333333,
0.566666666666667,0.6,0.633333333333333,0.666666666666667,0.7,0.733333333333333,
0.766666666666667,0.8,0.833333333333333,0.866666666666667,0.9,0.933333333333333,
0.966666666666667,1.),.UNSPECIFIED.)
CURVE()
GEOMETRIC_REPRESENTATION_ITEM()
RATIONAL_B_SPLINE_CURVE((1.,1.,1.,1.,1.,1.,1.,1.,1.,1.,1.,1.,1.,1.,1.,1.,
1.,1.,1.,1.,1.,1.,1.,1.,1.,1.,1.,1.,1.,1.,1.,1.,1.,1.,1.))
REPRESENTATION_ITEM('')
);
#193=(
BOUNDED_CURVE()
B_SPLINE_CURVE(5,(#10637,#10638,#10639,#10640,#10641,#10642,#10643,#10644,
#10645,#10646,#10647,#10648,#10649,#10650,#10651,#10652,#10653,#10654,#10655,
#10656,#10657,#10658,#10659,#10660,#10661,#10662,#10663,#10664,#10665,#10666,
#10667,#10668,#10669,#10670,#10671),.UNSPECIFIED.,.F.,.F.)
B_SPLINE_CURVE_WITH_KNOTS((6,1,1,1,1,1,1,1,1,1,1,1,1,1,1,1,1,1,1,1,1,1,
1,1,1,1,1,1,1,1,6),(0.,0.0333333333333333,0.0666666666666667,0.1,0.133333333333333,
0.166666666666667,0.2,0.233333333333333,0.266666666666667,0.3,0.333333333333333,
0.366666666666667,0.4,0.433333333333333,0.466666666666667,0.5,0.533333333333333,
0.566666666666667,0.6,0.633333333333333,0.666666666666667,0.7,0.733333333333333,
0.766666666666667,0.8,0.833333333333333,0.866666666666667,0.9,0.933333333333333,
0.966666666666667,1.),.UNSPECIFIED.)
CURVE()
GEOMETRIC_REPRESENTATION_ITEM()
RATIONAL_B_SPLINE_CURVE((1.,1.,1.,1.,1.,1.,1.,1.,1.,1.,1.,1.,1.,1.,1.,1.,
1.,1.,1.,1.,1.,1.,1.,1.,1.,1.,1.,1.,1.,1.,1.,1.,1.,1.,1.))
REPRESENTATION_ITEM('')
);
#194=(
BOUNDED_CURVE()
B_SPLINE_CURVE(5,(#10673,#10674,#10675,#10676,#10677,#10678,#10679,#10680,
#10681,#10682,#10683,#10684,#10685,#10686,#10687,#10688,#10689,#10690,#10691,
#10692,#10693,#10694,#10695,#10696,#10697,#10698,#10699,#10700,#10701,#10702,
#10703,#10704,#10705,#10706,#10707),.UNSPECIFIED.,.F.,.F.)
B_SPLINE_CURVE_WITH_KNOTS((6,1,1,1,1,1,1,1,1,1,1,1,1,1,1,1,1,1,1,1,1,1,
1,1,1,1,1,1,1,1,6),(0.,0.0333333333333333,0.0666666666666667,0.1,0.133333333333333,
0.166666666666667,0.2,0.233333333333333,0.266666666666667,0.3,0.333333333333333,
0.366666666666667,0.4,0.433333333333333,0.466666666666667,0.5,0.533333333333333,
0.566666666666667,0.6,0.633333333333333,0.666666666666667,0.7,0.733333333333333,
0.766666666666667,0.8,0.833333333333333,0.866666666666667,0.9,0.933333333333333,
0.966666666666667,1.),.UNSPECIFIED.)
CURVE()
GEOMETRIC_REPRESENTATION_ITEM()
RATIONAL_B_SPLINE_CURVE((1.,1.,1.,1.,1.,1.,1.,1.,1.,1.,1.,1.,1.,1.,1.,1.,
1.,1.,1.,1.,1.,1.,1.,1.,1.,1.,1.,1.,1.,1.,1.,1.,1.,1.,1.))
REPRESENTATION_ITEM('')
);
#195=(
BOUNDED_CURVE()
B_SPLINE_CURVE(5,(#10711,#10712,#10713,#10714,#10715,#10716,#10717,#10718,
#10719,#10720,#10721,#10722,#10723,#10724,#10725,#10726,#10727,#10728,#10729,
#10730,#10731,#10732,#10733,#10734,#10735,#10736,#10737,#10738,#10739,#10740,
#10741,#10742,#10743,#10744,#10745),.UNSPECIFIED.,.F.,.F.)
B_SPLINE_CURVE_WITH_KNOTS((6,1,1,1,1,1,1,1,1,1,1,1,1,1,1,1,1,1,1,1,1,1,
1,1,1,1,1,1,1,1,6),(0.,0.0333333333333333,0.0666666666666667,0.1,0.133333333333333,
0.166666666666667,0.2,0.233333333333333,0.266666666666667,0.3,0.333333333333333,
0.366666666666667,0.4,0.433333333333333,0.466666666666667,0.5,0.533333333333333,
0.566666666666667,0.6,0.633333333333333,0.666666666666667,0.7,0.733333333333333,
0.766666666666667,0.8,0.833333333333333,0.866666666666667,0.9,0.933333333333333,
0.966666666666667,1.),.UNSPECIFIED.)
CURVE()
GEOMETRIC_REPRESENTATION_ITEM()
RATIONAL_B_SPLINE_CURVE((1.,1.,1.,1.,1.,1.,1.,1.,1.,1.,1.,1.,1.,1.,1.,1.,
1.,1.,1.,1.,1.,1.,1.,1.,1.,1.,1.,1.,1.,1.,1.,1.,1.,1.,1.))
REPRESENTATION_ITEM('')
);
#196=(
BOUNDED_CURVE()
B_SPLINE_CURVE(5,(#10747,#10748,#10749,#10750,#10751,#10752,#10753,#10754,
#10755,#10756,#10757,#10758,#10759,#10760,#10761,#10762,#10763,#10764,#10765,
#10766,#10767,#10768,#10769,#10770,#10771,#10772,#10773,#10774,#10775,#10776,
#10777,#10778,#10779,#10780,#10781),.UNSPECIFIED.,.F.,.F.)
B_SPLINE_CURVE_WITH_KNOTS((6,1,1,1,1,1,1,1,1,1,1,1,1,1,1,1,1,1,1,1,1,1,
1,1,1,1,1,1,1,1,6),(0.,0.0333333333333333,0.0666666666666667,0.1,0.133333333333333,
0.166666666666667,0.2,0.233333333333333,0.266666666666667,0.3,0.333333333333333,
0.366666666666667,0.4,0.433333333333333,0.466666666666667,0.5,0.533333333333333,
0.566666666666667,0.6,0.633333333333333,0.666666666666667,0.7,0.733333333333333,
0.766666666666667,0.8,0.833333333333333,0.866666666666667,0.9,0.933333333333333,
0.966666666666667,1.),.UNSPECIFIED.)
CURVE()
GEOMETRIC_REPRESENTATION_ITEM()
RATIONAL_B_SPLINE_CURVE((1.,1.,1.,1.,1.,1.,1.,1.,1.,1.,1.,1.,1.,1.,1.,1.,
1.,1.,1.,1.,1.,1.,1.,1.,1.,1.,1.,1.,1.,1.,1.,1.,1.,1.,1.))
REPRESENTATION_ITEM('')
);
#197=(
BOUNDED_CURVE()
B_SPLINE_CURVE(5,(#10785,#10786,#10787,#10788,#10789,#10790,#10791,#10792,
#10793,#10794,#10795,#10796,#10797,#10798,#10799,#10800,#10801,#10802,#10803,
#10804,#10805,#10806,#10807,#10808,#10809,#10810,#10811,#10812,#10813,#10814,
#10815,#10816,#10817,#10818,#10819),.UNSPECIFIED.,.F.,.F.)
B_SPLINE_CURVE_WITH_KNOTS((6,1,1,1,1,1,1,1,1,1,1,1,1,1,1,1,1,1,1,1,1,1,
1,1,1,1,1,1,1,1,6),(0.,0.0333333333333333,0.0666666666666667,0.1,0.133333333333333,
0.166666666666667,0.2,0.233333333333333,0.266666666666667,0.3,0.333333333333333,
0.366666666666667,0.4,0.433333333333333,0.466666666666667,0.5,0.533333333333333,
0.566666666666667,0.6,0.633333333333333,0.666666666666667,0.7,0.733333333333333,
0.766666666666667,0.8,0.833333333333333,0.866666666666667,0.9,0.933333333333333,
0.966666666666667,1.),.UNSPECIFIED.)
CURVE()
GEOMETRIC_REPRESENTATION_ITEM()
RATIONAL_B_SPLINE_CURVE((1.,1.,1.,1.,1.,1.,1.,1.,1.,1.,1.,1.,1.,1.,1.,1.,
1.,1.,1.,1.,1.,1.,1.,1.,1.,1.,1.,1.,1.,1.,1.,1.,1.,1.,1.))
REPRESENTATION_ITEM('')
);
#198=(
BOUNDED_CURVE()
B_SPLINE_CURVE(5,(#10821,#10822,#10823,#10824,#10825,#10826,#10827,#10828,
#10829,#10830,#10831,#10832,#10833,#10834,#10835,#10836,#10837,#10838,#10839,
#10840,#10841,#10842,#10843,#10844,#10845,#10846,#10847,#10848,#10849,#10850,
#10851,#10852,#10853,#10854,#10855),.UNSPECIFIED.,.F.,.F.)
B_SPLINE_CURVE_WITH_KNOTS((6,1,1,1,1,1,1,1,1,1,1,1,1,1,1,1,1,1,1,1,1,1,
1,1,1,1,1,1,1,1,6),(0.,0.0333333333333333,0.0666666666666667,0.1,0.133333333333333,
0.166666666666667,0.2,0.233333333333333,0.266666666666667,0.3,0.333333333333333,
0.366666666666667,0.4,0.433333333333333,0.466666666666667,0.5,0.533333333333333,
0.566666666666667,0.6,0.633333333333333,0.666666666666667,0.7,0.733333333333333,
0.766666666666667,0.8,0.833333333333333,0.866666666666667,0.9,0.933333333333333,
0.966666666666667,1.),.UNSPECIFIED.)
CURVE()
GEOMETRIC_REPRESENTATION_ITEM()
RATIONAL_B_SPLINE_CURVE((1.,1.,1.,1.,1.,1.,1.,1.,1.,1.,1.,1.,1.,1.,1.,1.,
1.,1.,1.,1.,1.,1.,1.,1.,1.,1.,1.,1.,1.,1.,1.,1.,1.,1.,1.))
REPRESENTATION_ITEM('')
);
#199=(
BOUNDED_CURVE()
B_SPLINE_CURVE(5,(#10859,#10860,#10861,#10862,#10863,#10864,#10865,#10866,
#10867,#10868,#10869,#10870,#10871,#10872,#10873,#10874,#10875,#10876,#10877,
#10878,#10879,#10880,#10881,#10882,#10883,#10884,#10885,#10886,#10887,#10888,
#10889,#10890,#10891,#10892,#10893),.UNSPECIFIED.,.F.,.F.)
B_SPLINE_CURVE_WITH_KNOTS((6,1,1,1,1,1,1,1,1,1,1,1,1,1,1,1,1,1,1,1,1,1,
1,1,1,1,1,1,1,1,6),(0.,0.0333333333333333,0.0666666666666667,0.1,0.133333333333333,
0.166666666666667,0.2,0.233333333333333,0.266666666666667,0.3,0.333333333333333,
0.366666666666667,0.4,0.433333333333333,0.466666666666667,0.5,0.533333333333333,
0.566666666666667,0.6,0.633333333333333,0.666666666666667,0.7,0.733333333333333,
0.766666666666667,0.8,0.833333333333333,0.866666666666667,0.9,0.933333333333333,
0.966666666666667,1.),.UNSPECIFIED.)
CURVE()
GEOMETRIC_REPRESENTATION_ITEM()
RATIONAL_B_SPLINE_CURVE((1.,1.,1.,1.,1.,1.,1.,1.,1.,1.,1.,1.,1.,1.,1.,1.,
1.,1.,1.,1.,1.,1.,1.,1.,1.,1.,1.,1.,1.,1.,1.,1.,1.,1.,1.))
REPRESENTATION_ITEM('')
);
#200=(
BOUNDED_CURVE()
B_SPLINE_CURVE(5,(#10895,#10896,#10897,#10898,#10899,#10900,#10901,#10902,
#10903,#10904,#10905,#10906,#10907,#10908,#10909,#10910,#10911,#10912,#10913,
#10914,#10915,#10916,#10917,#10918,#10919,#10920,#10921,#10922,#10923,#10924,
#10925,#10926,#10927,#10928,#10929),.UNSPECIFIED.,.F.,.F.)
B_SPLINE_CURVE_WITH_KNOTS((6,1,1,1,1,1,1,1,1,1,1,1,1,1,1,1,1,1,1,1,1,1,
1,1,1,1,1,1,1,1,6),(0.,0.0333333333333333,0.0666666666666667,0.1,0.133333333333333,
0.166666666666667,0.2,0.233333333333333,0.266666666666667,0.3,0.333333333333333,
0.366666666666667,0.4,0.433333333333333,0.466666666666667,0.5,0.533333333333333,
0.566666666666667,0.6,0.633333333333333,0.666666666666667,0.7,0.733333333333333,
0.766666666666667,0.8,0.833333333333333,0.866666666666667,0.9,0.933333333333333,
0.966666666666667,1.),.UNSPECIFIED.)
CURVE()
GEOMETRIC_REPRESENTATION_ITEM()
RATIONAL_B_SPLINE_CURVE((1.,1.,1.,1.,1.,1.,1.,1.,1.,1.,1.,1.,1.,1.,1.,1.,
1.,1.,1.,1.,1.,1.,1.,1.,1.,1.,1.,1.,1.,1.,1.,1.,1.,1.,1.))
REPRESENTATION_ITEM('')
);
#201=(
BOUNDED_CURVE()
B_SPLINE_CURVE(5,(#10933,#10934,#10935,#10936,#10937,#10938,#10939,#10940,
#10941,#10942,#10943,#10944,#10945,#10946,#10947,#10948,#10949,#10950,#10951,
#10952,#10953,#10954,#10955,#10956,#10957,#10958,#10959,#10960,#10961,#10962,
#10963,#10964,#10965,#10966,#10967),.UNSPECIFIED.,.F.,.F.)
B_SPLINE_CURVE_WITH_KNOTS((6,1,1,1,1,1,1,1,1,1,1,1,1,1,1,1,1,1,1,1,1,1,
1,1,1,1,1,1,1,1,6),(0.,0.0333333333333333,0.0666666666666667,0.1,0.133333333333333,
0.166666666666667,0.2,0.233333333333333,0.266666666666667,0.3,0.333333333333333,
0.366666666666667,0.4,0.433333333333333,0.466666666666667,0.5,0.533333333333333,
0.566666666666667,0.6,0.633333333333333,0.666666666666667,0.7,0.733333333333333,
0.766666666666667,0.8,0.833333333333333,0.866666666666667,0.9,0.933333333333333,
0.966666666666667,1.),.UNSPECIFIED.)
CURVE()
GEOMETRIC_REPRESENTATION_ITEM()
RATIONAL_B_SPLINE_CURVE((1.,1.,1.,1.,1.,1.,1.,1.,1.,1.,1.,1.,1.,1.,1.,1.,
1.,1.,1.,1.,1.,1.,1.,1.,1.,1.,1.,1.,1.,1.,1.,1.,1.,1.,1.))
REPRESENTATION_ITEM('')
);
#202=(
BOUNDED_CURVE()
B_SPLINE_CURVE(5,(#10969,#10970,#10971,#10972,#10973,#10974,#10975,#10976,
#10977,#10978,#10979,#10980,#10981,#10982,#10983,#10984,#10985,#10986,#10987,
#10988,#10989,#10990,#10991,#10992,#10993,#10994,#10995,#10996,#10997,#10998,
#10999,#11000,#11001,#11002,#11003),.UNSPECIFIED.,.F.,.F.)
B_SPLINE_CURVE_WITH_KNOTS((6,1,1,1,1,1,1,1,1,1,1,1,1,1,1,1,1,1,1,1,1,1,
1,1,1,1,1,1,1,1,6),(0.,0.0333333333333333,0.0666666666666667,0.1,0.133333333333333,
0.166666666666667,0.2,0.233333333333333,0.266666666666667,0.3,0.333333333333333,
0.366666666666667,0.4,0.433333333333333,0.466666666666667,0.5,0.533333333333333,
0.566666666666667,0.6,0.633333333333333,0.666666666666667,0.7,0.733333333333333,
0.766666666666667,0.8,0.833333333333333,0.866666666666667,0.9,0.933333333333333,
0.966666666666667,1.),.UNSPECIFIED.)
CURVE()
GEOMETRIC_REPRESENTATION_ITEM()
RATIONAL_B_SPLINE_CURVE((1.,1.,1.,1.,1.,1.,1.,1.,1.,1.,1.,1.,1.,1.,1.,1.,
1.,1.,1.,1.,1.,1.,1.,1.,1.,1.,1.,1.,1.,1.,1.,1.,1.,1.,1.))
REPRESENTATION_ITEM('')
);
#203=(
BOUNDED_CURVE()
B_SPLINE_CURVE(5,(#11007,#11008,#11009,#11010,#11011,#11012,#11013,#11014,
#11015,#11016,#11017,#11018,#11019,#11020,#11021,#11022,#11023,#11024,#11025,
#11026,#11027,#11028,#11029,#11030,#11031,#11032,#11033,#11034,#11035,#11036,
#11037,#11038,#11039,#11040,#11041),.UNSPECIFIED.,.F.,.F.)
B_SPLINE_CURVE_WITH_KNOTS((6,1,1,1,1,1,1,1,1,1,1,1,1,1,1,1,1,1,1,1,1,1,
1,1,1,1,1,1,1,1,6),(0.,0.0333333333333333,0.0666666666666667,0.1,0.133333333333333,
0.166666666666667,0.2,0.233333333333333,0.266666666666667,0.3,0.333333333333333,
0.366666666666667,0.4,0.433333333333333,0.466666666666667,0.5,0.533333333333333,
0.566666666666667,0.6,0.633333333333333,0.666666666666667,0.7,0.733333333333333,
0.766666666666667,0.8,0.833333333333333,0.866666666666667,0.9,0.933333333333333,
0.966666666666667,1.),.UNSPECIFIED.)
CURVE()
GEOMETRIC_REPRESENTATION_ITEM()
RATIONAL_B_SPLINE_CURVE((1.,1.,1.,1.,1.,1.,1.,1.,1.,1.,1.,1.,1.,1.,1.,1.,
1.,1.,1.,1.,1.,1.,1.,1.,1.,1.,1.,1.,1.,1.,1.,1.,1.,1.,1.))
REPRESENTATION_ITEM('')
);
#204=(
BOUNDED_CURVE()
B_SPLINE_CURVE(5,(#11043,#11044,#11045,#11046,#11047,#11048,#11049,#11050,
#11051,#11052,#11053,#11054,#11055,#11056,#11057,#11058,#11059,#11060,#11061,
#11062,#11063,#11064,#11065,#11066,#11067,#11068,#11069,#11070,#11071,#11072,
#11073,#11074,#11075,#11076,#11077),.UNSPECIFIED.,.F.,.F.)
B_SPLINE_CURVE_WITH_KNOTS((6,1,1,1,1,1,1,1,1,1,1,1,1,1,1,1,1,1,1,1,1,1,
1,1,1,1,1,1,1,1,6),(0.,0.0333333333333333,0.0666666666666667,0.1,0.133333333333333,
0.166666666666667,0.2,0.233333333333333,0.266666666666667,0.3,0.333333333333333,
0.366666666666667,0.4,0.433333333333333,0.466666666666667,0.5,0.533333333333333,
0.566666666666667,0.6,0.633333333333333,0.666666666666667,0.7,0.733333333333333,
0.766666666666667,0.8,0.833333333333333,0.866666666666667,0.9,0.933333333333333,
0.966666666666667,1.),.UNSPECIFIED.)
CURVE()
GEOMETRIC_REPRESENTATION_ITEM()
RATIONAL_B_SPLINE_CURVE((1.,1.,1.,1.,1.,1.,1.,1.,1.,1.,1.,1.,1.,1.,1.,1.,
1.,1.,1.,1.,1.,1.,1.,1.,1.,1.,1.,1.,1.,1.,1.,1.,1.,1.,1.))
REPRESENTATION_ITEM('')
);
#205=(
BOUNDED_CURVE()
B_SPLINE_CURVE(5,(#11081,#11082,#11083,#11084,#11085,#11086,#11087,#11088,
#11089,#11090,#11091,#11092,#11093,#11094,#11095,#11096,#11097,#11098,#11099,
#11100,#11101,#11102,#11103,#11104,#11105,#11106,#11107,#11108,#11109,#11110,
#11111,#11112,#11113,#11114,#11115),.UNSPECIFIED.,.F.,.F.)
B_SPLINE_CURVE_WITH_KNOTS((6,1,1,1,1,1,1,1,1,1,1,1,1,1,1,1,1,1,1,1,1,1,
1,1,1,1,1,1,1,1,6),(0.,0.0333333333333333,0.0666666666666667,0.1,0.133333333333333,
0.166666666666667,0.2,0.233333333333333,0.266666666666667,0.3,0.333333333333333,
0.366666666666667,0.4,0.433333333333333,0.466666666666667,0.5,0.533333333333333,
0.566666666666667,0.6,0.633333333333333,0.666666666666667,0.7,0.733333333333333,
0.766666666666667,0.8,0.833333333333333,0.866666666666667,0.9,0.933333333333333,
0.966666666666667,1.),.UNSPECIFIED.)
CURVE()
GEOMETRIC_REPRESENTATION_ITEM()
RATIONAL_B_SPLINE_CURVE((1.,1.,1.,1.,1.,1.,1.,1.,1.,1.,1.,1.,1.,1.,1.,1.,
1.,1.,1.,1.,1.,1.,1.,1.,1.,1.,1.,1.,1.,1.,1.,1.,1.,1.,1.))
REPRESENTATION_ITEM('')
);
#206=(
BOUNDED_CURVE()
B_SPLINE_CURVE(5,(#11117,#11118,#11119,#11120,#11121,#11122,#11123,#11124,
#11125,#11126,#11127,#11128,#11129,#11130,#11131,#11132,#11133,#11134,#11135,
#11136,#11137,#11138,#11139,#11140,#11141,#11142,#11143,#11144,#11145,#11146,
#11147,#11148,#11149,#11150,#11151),.UNSPECIFIED.,.F.,.F.)
B_SPLINE_CURVE_WITH_KNOTS((6,1,1,1,1,1,1,1,1,1,1,1,1,1,1,1,1,1,1,1,1,1,
1,1,1,1,1,1,1,1,6),(0.,0.0333333333333333,0.0666666666666667,0.1,0.133333333333333,
0.166666666666667,0.2,0.233333333333333,0.266666666666667,0.3,0.333333333333333,
0.366666666666667,0.4,0.433333333333333,0.466666666666667,0.5,0.533333333333333,
0.566666666666667,0.6,0.633333333333333,0.666666666666667,0.7,0.733333333333333,
0.766666666666667,0.8,0.833333333333333,0.866666666666667,0.9,0.933333333333333,
0.966666666666667,1.),.UNSPECIFIED.)
CURVE()
GEOMETRIC_REPRESENTATION_ITEM()
RATIONAL_B_SPLINE_CURVE((1.,1.,1.,1.,1.,1.,1.,1.,1.,1.,1.,1.,1.,1.,1.,1.,
1.,1.,1.,1.,1.,1.,1.,1.,1.,1.,1.,1.,1.,1.,1.,1.,1.,1.,1.))
REPRESENTATION_ITEM('')
);
#207=(
BOUNDED_CURVE()
B_SPLINE_CURVE(5,(#11155,#11156,#11157,#11158,#11159,#11160,#11161,#11162,
#11163,#11164,#11165,#11166,#11167,#11168,#11169,#11170,#11171,#11172,#11173,
#11174,#11175,#11176,#11177,#11178,#11179,#11180,#11181,#11182,#11183,#11184,
#11185,#11186,#11187,#11188,#11189),.UNSPECIFIED.,.F.,.F.)
B_SPLINE_CURVE_WITH_KNOTS((6,1,1,1,1,1,1,1,1,1,1,1,1,1,1,1,1,1,1,1,1,1,
1,1,1,1,1,1,1,1,6),(0.,0.0333333333333333,0.0666666666666667,0.1,0.133333333333333,
0.166666666666667,0.2,0.233333333333333,0.266666666666667,0.3,0.333333333333333,
0.366666666666667,0.4,0.433333333333333,0.466666666666667,0.5,0.533333333333333,
0.566666666666667,0.6,0.633333333333333,0.666666666666667,0.7,0.733333333333333,
0.766666666666667,0.8,0.833333333333333,0.866666666666667,0.9,0.933333333333333,
0.966666666666667,1.),.UNSPECIFIED.)
CURVE()
GEOMETRIC_REPRESENTATION_ITEM()
RATIONAL_B_SPLINE_CURVE((1.,1.,1.,1.,1.,1.,1.,1.,1.,1.,1.,1.,1.,1.,1.,1.,
1.,1.,1.,1.,1.,1.,1.,1.,1.,1.,1.,1.,1.,1.,1.,1.,1.,1.,1.))
REPRESENTATION_ITEM('')
);
#208=(
BOUNDED_CURVE()
B_SPLINE_CURVE(5,(#11191,#11192,#11193,#11194,#11195,#11196,#11197,#11198,
#11199,#11200,#11201,#11202,#11203,#11204,#11205,#11206,#11207,#11208,#11209,
#11210,#11211,#11212,#11213,#11214,#11215,#11216,#11217,#11218,#11219,#11220,
#11221,#11222,#11223,#11224,#11225),.UNSPECIFIED.,.F.,.F.)
B_SPLINE_CURVE_WITH_KNOTS((6,1,1,1,1,1,1,1,1,1,1,1,1,1,1,1,1,1,1,1,1,1,
1,1,1,1,1,1,1,1,6),(0.,0.0333333333333333,0.0666666666666667,0.1,0.133333333333333,
0.166666666666667,0.2,0.233333333333333,0.266666666666667,0.3,0.333333333333333,
0.366666666666667,0.4,0.433333333333333,0.466666666666667,0.5,0.533333333333333,
0.566666666666667,0.6,0.633333333333333,0.666666666666667,0.7,0.733333333333333,
0.766666666666667,0.8,0.833333333333333,0.866666666666667,0.9,0.933333333333333,
0.966666666666667,1.),.UNSPECIFIED.)
CURVE()
GEOMETRIC_REPRESENTATION_ITEM()
RATIONAL_B_SPLINE_CURVE((1.,1.,1.,1.,1.,1.,1.,1.,1.,1.,1.,1.,1.,1.,1.,1.,
1.,1.,1.,1.,1.,1.,1.,1.,1.,1.,1.,1.,1.,1.,1.,1.,1.,1.,1.))
REPRESENTATION_ITEM('')
);
#209=(
BOUNDED_CURVE()
B_SPLINE_CURVE(5,(#11229,#11230,#11231,#11232,#11233,#11234,#11235,#11236,
#11237,#11238,#11239,#11240,#11241,#11242,#11243,#11244,#11245,#11246,#11247,
#11248,#11249,#11250,#11251,#11252,#11253,#11254,#11255,#11256,#11257,#11258,
#11259,#11260,#11261,#11262,#11263),.UNSPECIFIED.,.F.,.F.)
B_SPLINE_CURVE_WITH_KNOTS((6,1,1,1,1,1,1,1,1,1,1,1,1,1,1,1,1,1,1,1,1,1,
1,1,1,1,1,1,1,1,6),(0.,0.0333333333333333,0.0666666666666667,0.1,0.133333333333333,
0.166666666666667,0.2,0.233333333333333,0.266666666666667,0.3,0.333333333333333,
0.366666666666667,0.4,0.433333333333333,0.466666666666667,0.5,0.533333333333333,
0.566666666666667,0.6,0.633333333333333,0.666666666666667,0.7,0.733333333333333,
0.766666666666667,0.8,0.833333333333333,0.866666666666667,0.9,0.933333333333333,
0.966666666666667,1.),.UNSPECIFIED.)
CURVE()
GEOMETRIC_REPRESENTATION_ITEM()
RATIONAL_B_SPLINE_CURVE((1.,1.,1.,1.,1.,1.,1.,1.,1.,1.,1.,1.,1.,1.,1.,1.,
1.,1.,1.,1.,1.,1.,1.,1.,1.,1.,1.,1.,1.,1.,1.,1.,1.,1.,1.))
REPRESENTATION_ITEM('')
);
#210=(
BOUNDED_CURVE()
B_SPLINE_CURVE(5,(#11265,#11266,#11267,#11268,#11269,#11270,#11271,#11272,
#11273,#11274,#11275,#11276,#11277,#11278,#11279,#11280,#11281,#11282,#11283,
#11284,#11285,#11286,#11287,#11288,#11289,#11290,#11291,#11292,#11293,#11294,
#11295,#11296,#11297,#11298,#11299),.UNSPECIFIED.,.F.,.F.)
B_SPLINE_CURVE_WITH_KNOTS((6,1,1,1,1,1,1,1,1,1,1,1,1,1,1,1,1,1,1,1,1,1,
1,1,1,1,1,1,1,1,6),(0.,0.0333333333333333,0.0666666666666667,0.1,0.133333333333333,
0.166666666666667,0.2,0.233333333333333,0.266666666666667,0.3,0.333333333333333,
0.366666666666667,0.4,0.433333333333333,0.466666666666667,0.5,0.533333333333333,
0.566666666666667,0.6,0.633333333333333,0.666666666666667,0.7,0.733333333333333,
0.766666666666667,0.8,0.833333333333333,0.866666666666667,0.9,0.933333333333333,
0.966666666666667,1.),.UNSPECIFIED.)
CURVE()
GEOMETRIC_REPRESENTATION_ITEM()
RATIONAL_B_SPLINE_CURVE((1.,1.,1.,1.,1.,1.,1.,1.,1.,1.,1.,1.,1.,1.,1.,1.,
1.,1.,1.,1.,1.,1.,1.,1.,1.,1.,1.,1.,1.,1.,1.,1.,1.,1.,1.))
REPRESENTATION_ITEM('')
);
#211=(
BOUNDED_CURVE()
B_SPLINE_CURVE(5,(#11303,#11304,#11305,#11306,#11307,#11308,#11309,#11310,
#11311,#11312,#11313,#11314,#11315,#11316,#11317,#11318,#11319,#11320,#11321,
#11322,#11323,#11324,#11325,#11326,#11327,#11328,#11329,#11330,#11331,#11332,
#11333,#11334,#11335,#11336,#11337),.UNSPECIFIED.,.F.,.F.)
B_SPLINE_CURVE_WITH_KNOTS((6,1,1,1,1,1,1,1,1,1,1,1,1,1,1,1,1,1,1,1,1,1,
1,1,1,1,1,1,1,1,6),(0.,0.0333333333333333,0.0666666666666667,0.1,0.133333333333333,
0.166666666666667,0.2,0.233333333333333,0.266666666666667,0.3,0.333333333333333,
0.366666666666667,0.4,0.433333333333333,0.466666666666667,0.5,0.533333333333333,
0.566666666666667,0.6,0.633333333333333,0.666666666666667,0.7,0.733333333333333,
0.766666666666667,0.8,0.833333333333333,0.866666666666667,0.9,0.933333333333333,
0.966666666666667,1.),.UNSPECIFIED.)
CURVE()
GEOMETRIC_REPRESENTATION_ITEM()
RATIONAL_B_SPLINE_CURVE((1.,1.,1.,1.,1.,1.,1.,1.,1.,1.,1.,1.,1.,1.,1.,1.,
1.,1.,1.,1.,1.,1.,1.,1.,1.,1.,1.,1.,1.,1.,1.,1.,1.,1.,1.))
REPRESENTATION_ITEM('')
);
#212=(
BOUNDED_CURVE()
B_SPLINE_CURVE(5,(#11339,#11340,#11341,#11342,#11343,#11344,#11345,#11346,
#11347,#11348,#11349,#11350,#11351,#11352,#11353,#11354,#11355,#11356,#11357,
#11358,#11359,#11360,#11361,#11362,#11363,#11364,#11365,#11366,#11367,#11368,
#11369,#11370,#11371,#11372,#11373),.UNSPECIFIED.,.F.,.F.)
B_SPLINE_CURVE_WITH_KNOTS((6,1,1,1,1,1,1,1,1,1,1,1,1,1,1,1,1,1,1,1,1,1,
1,1,1,1,1,1,1,1,6),(0.,0.0333333333333333,0.0666666666666667,0.1,0.133333333333333,
0.166666666666667,0.2,0.233333333333333,0.266666666666667,0.3,0.333333333333333,
0.366666666666667,0.4,0.433333333333333,0.466666666666667,0.5,0.533333333333333,
0.566666666666667,0.6,0.633333333333333,0.666666666666667,0.7,0.733333333333333,
0.766666666666667,0.8,0.833333333333333,0.866666666666667,0.9,0.933333333333333,
0.966666666666667,1.),.UNSPECIFIED.)
CURVE()
GEOMETRIC_REPRESENTATION_ITEM()
RATIONAL_B_SPLINE_CURVE((1.,1.,1.,1.,1.,1.,1.,1.,1.,1.,1.,1.,1.,1.,1.,1.,
1.,1.,1.,1.,1.,1.,1.,1.,1.,1.,1.,1.,1.,1.,1.,1.,1.,1.,1.))
REPRESENTATION_ITEM('')
);
#213=(
BOUNDED_CURVE()
B_SPLINE_CURVE(5,(#11377,#11378,#11379,#11380,#11381,#11382,#11383,#11384,
#11385,#11386,#11387,#11388,#11389,#11390,#11391,#11392,#11393,#11394,#11395,
#11396,#11397,#11398,#11399,#11400,#11401,#11402,#11403,#11404,#11405,#11406,
#11407,#11408,#11409,#11410,#11411),.UNSPECIFIED.,.F.,.F.)
B_SPLINE_CURVE_WITH_KNOTS((6,1,1,1,1,1,1,1,1,1,1,1,1,1,1,1,1,1,1,1,1,1,
1,1,1,1,1,1,1,1,6),(0.,0.0333333333333333,0.0666666666666667,0.1,0.133333333333333,
0.166666666666667,0.2,0.233333333333333,0.266666666666667,0.3,0.333333333333333,
0.366666666666667,0.4,0.433333333333333,0.466666666666667,0.5,0.533333333333333,
0.566666666666667,0.6,0.633333333333333,0.666666666666667,0.7,0.733333333333333,
0.766666666666667,0.8,0.833333333333333,0.866666666666667,0.9,0.933333333333333,
0.966666666666667,1.),.UNSPECIFIED.)
CURVE()
GEOMETRIC_REPRESENTATION_ITEM()
RATIONAL_B_SPLINE_CURVE((1.,1.,1.,1.,1.,1.,1.,1.,1.,1.,1.,1.,1.,1.,1.,1.,
1.,1.,1.,1.,1.,1.,1.,1.,1.,1.,1.,1.,1.,1.,1.,1.,1.,1.,1.))
REPRESENTATION_ITEM('')
);
#214=(
BOUNDED_CURVE()
B_SPLINE_CURVE(5,(#11412,#11413,#11414,#11415,#11416,#11417,#11418,#11419,
#11420,#11421,#11422,#11423,#11424,#11425,#11426,#11427,#11428,#11429,#11430,
#11431,#11432,#11433,#11434,#11435,#11436,#11437,#11438,#11439,#11440,#11441,
#11442,#11443,#11444,#11445,#11446),.UNSPECIFIED.,.F.,.F.)
B_SPLINE_CURVE_WITH_KNOTS((6,1,1,1,1,1,1,1,1,1,1,1,1,1,1,1,1,1,1,1,1,1,
1,1,1,1,1,1,1,1,6),(0.,0.0333333333333333,0.0666666666666667,0.1,0.133333333333333,
0.166666666666667,0.2,0.233333333333333,0.266666666666667,0.3,0.333333333333333,
0.366666666666667,0.4,0.433333333333333,0.466666666666667,0.5,0.533333333333333,
0.566666666666667,0.6,0.633333333333333,0.666666666666667,0.7,0.733333333333333,
0.766666666666667,0.8,0.833333333333333,0.866666666666667,0.9,0.933333333333333,
0.966666666666667,1.),.UNSPECIFIED.)
CURVE()
GEOMETRIC_REPRESENTATION_ITEM()
RATIONAL_B_SPLINE_CURVE((1.,1.,1.,1.,1.,1.,1.,1.,1.,1.,1.,1.,1.,1.,1.,1.,
1.,1.,1.,1.,1.,1.,1.,1.,1.,1.,1.,1.,1.,1.,1.,1.,1.,1.,1.))
REPRESENTATION_ITEM('')
);
#215=(
BOUNDED_CURVE()
B_SPLINE_CURVE(5,(#12149,#12150,#12151,#12152,#12153,#12154),
 .UNSPECIFIED.,.F.,.F.)
B_SPLINE_CURVE_WITH_KNOTS((6,6),(0.,0.0167044419747604),.UNSPECIFIED.)
CURVE()
GEOMETRIC_REPRESENTATION_ITEM()
RATIONAL_B_SPLINE_CURVE((1.,1.,1.,1.,1.,1.))
REPRESENTATION_ITEM('')
);
#216=(
BOUNDED_CURVE()
B_SPLINE_CURVE(5,(#12209,#12210,#12211,#12212,#12213,#12214),
 .UNSPECIFIED.,.F.,.F.)
B_SPLINE_CURVE_WITH_KNOTS((6,6),(0.,0.0167044419747598),.UNSPECIFIED.)
CURVE()
GEOMETRIC_REPRESENTATION_ITEM()
RATIONAL_B_SPLINE_CURVE((1.,1.,1.,1.,1.,1.))
REPRESENTATION_ITEM('')
);
#217=(
BOUNDED_CURVE()
B_SPLINE_CURVE(5,(#12269,#12270,#12271,#12272,#12273,#12274),
 .UNSPECIFIED.,.F.,.F.)
B_SPLINE_CURVE_WITH_KNOTS((6,6),(0.,0.0167044419747601),.UNSPECIFIED.)
CURVE()
GEOMETRIC_REPRESENTATION_ITEM()
RATIONAL_B_SPLINE_CURVE((1.,1.,1.,1.,1.,1.))
REPRESENTATION_ITEM('')
);
#218=(
BOUNDED_CURVE()
B_SPLINE_CURVE(5,(#12329,#12330,#12331,#12332,#12333,#12334),
 .UNSPECIFIED.,.F.,.F.)
B_SPLINE_CURVE_WITH_KNOTS((6,6),(0.,0.0167044419747607),.UNSPECIFIED.)
CURVE()
GEOMETRIC_REPRESENTATION_ITEM()
RATIONAL_B_SPLINE_CURVE((1.,1.,1.,1.,1.,1.))
REPRESENTATION_ITEM('')
);
#219=(
BOUNDED_CURVE()
B_SPLINE_CURVE(5,(#12389,#12390,#12391,#12392,#12393,#12394),
 .UNSPECIFIED.,.F.,.F.)
B_SPLINE_CURVE_WITH_KNOTS((6,6),(0.,0.0167044419747605),.UNSPECIFIED.)
CURVE()
GEOMETRIC_REPRESENTATION_ITEM()
RATIONAL_B_SPLINE_CURVE((1.,1.,1.,1.,1.,1.))
REPRESENTATION_ITEM('')
);
#220=(
BOUNDED_CURVE()
B_SPLINE_CURVE(5,(#12449,#12450,#12451,#12452,#12453,#12454),
 .UNSPECIFIED.,.F.,.F.)
B_SPLINE_CURVE_WITH_KNOTS((6,6),(0.,0.0167044419747612),.UNSPECIFIED.)
CURVE()
GEOMETRIC_REPRESENTATION_ITEM()
RATIONAL_B_SPLINE_CURVE((1.,1.,1.,1.,1.,1.))
REPRESENTATION_ITEM('')
);
#221=(
BOUNDED_CURVE()
B_SPLINE_CURVE(5,(#12509,#12510,#12511,#12512,#12513,#12514),
 .UNSPECIFIED.,.F.,.F.)
B_SPLINE_CURVE_WITH_KNOTS((6,6),(0.,0.01670444197476),.UNSPECIFIED.)
CURVE()
GEOMETRIC_REPRESENTATION_ITEM()
RATIONAL_B_SPLINE_CURVE((1.,1.,1.,1.,1.,1.))
REPRESENTATION_ITEM('')
);
#222=(
BOUNDED_CURVE()
B_SPLINE_CURVE(5,(#12569,#12570,#12571,#12572,#12573,#12574),
 .UNSPECIFIED.,.F.,.F.)
B_SPLINE_CURVE_WITH_KNOTS((6,6),(0.,0.0167044419747599),.UNSPECIFIED.)
CURVE()
GEOMETRIC_REPRESENTATION_ITEM()
RATIONAL_B_SPLINE_CURVE((1.,1.,1.,1.,1.,1.))
REPRESENTATION_ITEM('')
);
#223=(
BOUNDED_CURVE()
B_SPLINE_CURVE(5,(#12629,#12630,#12631,#12632,#12633,#12634),
 .UNSPECIFIED.,.F.,.F.)
B_SPLINE_CURVE_WITH_KNOTS((6,6),(0.,0.01670444197476),.UNSPECIFIED.)
CURVE()
GEOMETRIC_REPRESENTATION_ITEM()
RATIONAL_B_SPLINE_CURVE((1.,1.,1.,1.,1.,1.))
REPRESENTATION_ITEM('')
);
#224=(
BOUNDED_CURVE()
B_SPLINE_CURVE(5,(#12689,#12690,#12691,#12692,#12693,#12694),
 .UNSPECIFIED.,.F.,.F.)
B_SPLINE_CURVE_WITH_KNOTS((6,6),(0.,0.0167044419747604),.UNSPECIFIED.)
CURVE()
GEOMETRIC_REPRESENTATION_ITEM()
RATIONAL_B_SPLINE_CURVE((1.,1.,1.,1.,1.,1.))
REPRESENTATION_ITEM('')
);
#225=(
BOUNDED_CURVE()
B_SPLINE_CURVE(5,(#12725,#12726,#12727,#12728,#12729,#12730),
 .UNSPECIFIED.,.F.,.F.)
B_SPLINE_CURVE_WITH_KNOTS((6,6),(0.,0.0167044419747612),.UNSPECIFIED.)
CURVE()
GEOMETRIC_REPRESENTATION_ITEM()
RATIONAL_B_SPLINE_CURVE((1.,1.,1.,1.,1.,1.))
REPRESENTATION_ITEM('')
);
#226=(
BOUNDED_CURVE()
B_SPLINE_CURVE(5,(#12785,#12786,#12787,#12788,#12789,#12790),
 .UNSPECIFIED.,.F.,.F.)
B_SPLINE_CURVE_WITH_KNOTS((6,6),(0.,0.01670444197476),.UNSPECIFIED.)
CURVE()
GEOMETRIC_REPRESENTATION_ITEM()
RATIONAL_B_SPLINE_CURVE((1.,1.,1.,1.,1.,1.))
REPRESENTATION_ITEM('')
);
#227=(
BOUNDED_CURVE()
B_SPLINE_CURVE(5,(#12845,#12846,#12847,#12848,#12849,#12850),
 .UNSPECIFIED.,.F.,.F.)
B_SPLINE_CURVE_WITH_KNOTS((6,6),(0.,0.0167044419747599),.UNSPECIFIED.)
CURVE()
GEOMETRIC_REPRESENTATION_ITEM()
RATIONAL_B_SPLINE_CURVE((1.,1.,1.,1.,1.,1.))
REPRESENTATION_ITEM('')
);
#228=(
BOUNDED_CURVE()
B_SPLINE_CURVE(5,(#12905,#12906,#12907,#12908,#12909,#12910),
 .UNSPECIFIED.,.F.,.F.)
B_SPLINE_CURVE_WITH_KNOTS((6,6),(0.,0.01670444197476),.UNSPECIFIED.)
CURVE()
GEOMETRIC_REPRESENTATION_ITEM()
RATIONAL_B_SPLINE_CURVE((1.,1.,1.,1.,1.,1.))
REPRESENTATION_ITEM('')
);
#229=(
BOUNDED_CURVE()
B_SPLINE_CURVE(5,(#12965,#12966,#12967,#12968,#12969,#12970),
 .UNSPECIFIED.,.F.,.F.)
B_SPLINE_CURVE_WITH_KNOTS((6,6),(0.,0.0167044419747602),.UNSPECIFIED.)
CURVE()
GEOMETRIC_REPRESENTATION_ITEM()
RATIONAL_B_SPLINE_CURVE((1.,1.,1.,1.,1.,1.))
REPRESENTATION_ITEM('')
);
#230=(
BOUNDED_CURVE()
B_SPLINE_CURVE(5,(#13025,#13026,#13027,#13028,#13029,#13030),
 .UNSPECIFIED.,.F.,.F.)
B_SPLINE_CURVE_WITH_KNOTS((6,6),(0.,0.0167044419747598),.UNSPECIFIED.)
CURVE()
GEOMETRIC_REPRESENTATION_ITEM()
RATIONAL_B_SPLINE_CURVE((1.,1.,1.,1.,1.,1.))
REPRESENTATION_ITEM('')
);
#231=(
BOUNDED_CURVE()
B_SPLINE_CURVE(5,(#13085,#13086,#13087,#13088,#13089,#13090),
 .UNSPECIFIED.,.F.,.F.)
B_SPLINE_CURVE_WITH_KNOTS((6,6),(0.,0.0167044419747605),.UNSPECIFIED.)
CURVE()
GEOMETRIC_REPRESENTATION_ITEM()
RATIONAL_B_SPLINE_CURVE((1.,1.,1.,1.,1.,1.))
REPRESENTATION_ITEM('')
);
#232=(
BOUNDED_CURVE()
B_SPLINE_CURVE(5,(#13145,#13146,#13147,#13148,#13149,#13150),
 .UNSPECIFIED.,.F.,.F.)
B_SPLINE_CURVE_WITH_KNOTS((6,6),(0.,0.0167044419747605),.UNSPECIFIED.)
CURVE()
GEOMETRIC_REPRESENTATION_ITEM()
RATIONAL_B_SPLINE_CURVE((1.,1.,1.,1.,1.,1.))
REPRESENTATION_ITEM('')
);
#233=(
BOUNDED_CURVE()
B_SPLINE_CURVE(5,(#13205,#13206,#13207,#13208,#13209,#13210),
 .UNSPECIFIED.,.F.,.F.)
B_SPLINE_CURVE_WITH_KNOTS((6,6),(0.,0.0167044419747594),.UNSPECIFIED.)
CURVE()
GEOMETRIC_REPRESENTATION_ITEM()
RATIONAL_B_SPLINE_CURVE((1.,1.,1.,1.,1.,1.))
REPRESENTATION_ITEM('')
);
#234=(
BOUNDED_CURVE()
B_SPLINE_CURVE(5,(#13265,#13266,#13267,#13268,#13269,#13270),
 .UNSPECIFIED.,.F.,.F.)
B_SPLINE_CURVE_WITH_KNOTS((6,6),(0.,0.0167044419747601),.UNSPECIFIED.)
CURVE()
GEOMETRIC_REPRESENTATION_ITEM()
RATIONAL_B_SPLINE_CURVE((1.,1.,1.,1.,1.,1.))
REPRESENTATION_ITEM('')
);
#235=(
BOUNDED_CURVE()
B_SPLINE_CURVE(5,(#13382,#13383,#13384,#13385,#13386,#13387),
 .UNSPECIFIED.,.F.,.F.)
B_SPLINE_CURVE_WITH_KNOTS((6,6),(0.984324037881406,1.),.UNSPECIFIED.)
CURVE()
GEOMETRIC_REPRESENTATION_ITEM()
RATIONAL_B_SPLINE_CURVE((1.,1.,1.,1.,1.,1.))
REPRESENTATION_ITEM('')
);
#236=(
BOUNDED_CURVE()
B_SPLINE_CURVE(5,(#14224,#14225,#14226,#14227,#14228,#14229),
 .UNSPECIFIED.,.F.,.F.)
B_SPLINE_CURVE_WITH_KNOTS((6,6),(0.984324037881406,1.),.UNSPECIFIED.)
CURVE()
GEOMETRIC_REPRESENTATION_ITEM()
RATIONAL_B_SPLINE_CURVE((1.,1.,1.,1.,1.,1.))
REPRESENTATION_ITEM('')
);
#237=(
BOUNDED_CURVE()
B_SPLINE_CURVE(5,(#14341,#14342,#14343,#14344,#14345,#14346),
 .UNSPECIFIED.,.F.,.F.)
B_SPLINE_CURVE_WITH_KNOTS((6,6),(0.984324037881405,1.),.UNSPECIFIED.)
CURVE()
GEOMETRIC_REPRESENTATION_ITEM()
RATIONAL_B_SPLINE_CURVE((1.,1.,1.,1.,1.,1.))
REPRESENTATION_ITEM('')
);
#238=(
BOUNDED_CURVE()
B_SPLINE_CURVE(5,(#14396,#14397,#14398,#14399,#14400,#14401),
 .UNSPECIFIED.,.F.,.F.)
B_SPLINE_CURVE_WITH_KNOTS((6,6),(0.984324037881405,1.),.UNSPECIFIED.)
CURVE()
GEOMETRIC_REPRESENTATION_ITEM()
RATIONAL_B_SPLINE_CURVE((1.,1.,1.,1.,1.,1.))
REPRESENTATION_ITEM('')
);
#239=(
BOUNDED_CURVE()
B_SPLINE_CURVE(5,(#14451,#14452,#14453,#14454,#14455,#14456),
 .UNSPECIFIED.,.F.,.F.)
B_SPLINE_CURVE_WITH_KNOTS((6,6),(0.984324037881405,1.),.UNSPECIFIED.)
CURVE()
GEOMETRIC_REPRESENTATION_ITEM()
RATIONAL_B_SPLINE_CURVE((1.,1.,1.,1.,1.,1.))
REPRESENTATION_ITEM('')
);
#240=(
BOUNDED_CURVE()
B_SPLINE_CURVE(5,(#14568,#14569,#14570,#14571,#14572,#14573),
 .UNSPECIFIED.,.F.,.F.)
B_SPLINE_CURVE_WITH_KNOTS((6,6),(0.984324037881406,1.),.UNSPECIFIED.)
CURVE()
GEOMETRIC_REPRESENTATION_ITEM()
RATIONAL_B_SPLINE_CURVE((1.,1.,1.,1.,1.,1.))
REPRESENTATION_ITEM('')
);
#241=(
BOUNDED_CURVE()
B_SPLINE_CURVE(5,(#14685,#14686,#14687,#14688,#14689,#14690),
 .UNSPECIFIED.,.F.,.F.)
B_SPLINE_CURVE_WITH_KNOTS((6,6),(0.984324037881406,1.),.UNSPECIFIED.)
CURVE()
GEOMETRIC_REPRESENTATION_ITEM()
RATIONAL_B_SPLINE_CURVE((1.,1.,1.,1.,1.,1.))
REPRESENTATION_ITEM('')
);
#242=(
BOUNDED_CURVE()
B_SPLINE_CURVE(5,(#14802,#14803,#14804,#14805,#14806,#14807),
 .UNSPECIFIED.,.F.,.F.)
B_SPLINE_CURVE_WITH_KNOTS((6,6),(0.984324037881406,1.),.UNSPECIFIED.)
CURVE()
GEOMETRIC_REPRESENTATION_ITEM()
RATIONAL_B_SPLINE_CURVE((1.,1.,1.,1.,1.,1.))
REPRESENTATION_ITEM('')
);
#243=(
BOUNDED_CURVE()
B_SPLINE_CURVE(5,(#14857,#14858,#14859,#14860,#14861,#14862),
 .UNSPECIFIED.,.F.,.F.)
B_SPLINE_CURVE_WITH_KNOTS((6,6),(0.984324037881405,1.),.UNSPECIFIED.)
CURVE()
GEOMETRIC_REPRESENTATION_ITEM()
RATIONAL_B_SPLINE_CURVE((1.,1.,1.,1.,1.,1.))
REPRESENTATION_ITEM('')
);
#244=(
BOUNDED_CURVE()
B_SPLINE_CURVE(5,(#14912,#14913,#14914,#14915,#14916,#14917),
 .UNSPECIFIED.,.F.,.F.)
B_SPLINE_CURVE_WITH_KNOTS((6,6),(0.984324037881405,1.),.UNSPECIFIED.)
CURVE()
GEOMETRIC_REPRESENTATION_ITEM()
RATIONAL_B_SPLINE_CURVE((1.,1.,1.,1.,1.,1.))
REPRESENTATION_ITEM('')
);
#245=(
BOUNDED_CURVE()
B_SPLINE_CURVE(5,(#15029,#15030,#15031,#15032,#15033,#15034),
 .UNSPECIFIED.,.F.,.F.)
B_SPLINE_CURVE_WITH_KNOTS((6,6),(0.984324037881406,1.),.UNSPECIFIED.)
CURVE()
GEOMETRIC_REPRESENTATION_ITEM()
RATIONAL_B_SPLINE_CURVE((1.,1.,1.,1.,1.,1.))
REPRESENTATION_ITEM('')
);
#246=(
BOUNDED_CURVE()
B_SPLINE_CURVE(5,(#15146,#15147,#15148,#15149,#15150,#15151),
 .UNSPECIFIED.,.F.,.F.)
B_SPLINE_CURVE_WITH_KNOTS((6,6),(0.984324037881406,1.),.UNSPECIFIED.)
CURVE()
GEOMETRIC_REPRESENTATION_ITEM()
RATIONAL_B_SPLINE_CURVE((1.,1.,1.,1.,1.,1.))
REPRESENTATION_ITEM('')
);
#247=(
BOUNDED_CURVE()
B_SPLINE_CURVE(5,(#15263,#15264,#15265,#15266,#15267,#15268),
 .UNSPECIFIED.,.F.,.F.)
B_SPLINE_CURVE_WITH_KNOTS((6,6),(0.984324037881406,1.),.UNSPECIFIED.)
CURVE()
GEOMETRIC_REPRESENTATION_ITEM()
RATIONAL_B_SPLINE_CURVE((1.,1.,1.,1.,1.,1.))
REPRESENTATION_ITEM('')
);
#248=(
BOUNDED_CURVE()
B_SPLINE_CURVE(5,(#15318,#15319,#15320,#15321,#15322,#15323),
 .UNSPECIFIED.,.F.,.F.)
B_SPLINE_CURVE_WITH_KNOTS((6,6),(0.984324037881405,1.),.UNSPECIFIED.)
CURVE()
GEOMETRIC_REPRESENTATION_ITEM()
RATIONAL_B_SPLINE_CURVE((1.,1.,1.,1.,1.,1.))
REPRESENTATION_ITEM('')
);
#249=(
BOUNDED_CURVE()
B_SPLINE_CURVE(5,(#15373,#15374,#15375,#15376,#15377,#15378),
 .UNSPECIFIED.,.F.,.F.)
B_SPLINE_CURVE_WITH_KNOTS((6,6),(0.984324037881405,1.),.UNSPECIFIED.)
CURVE()
GEOMETRIC_REPRESENTATION_ITEM()
RATIONAL_B_SPLINE_CURVE((1.,1.,1.,1.,1.,1.))
REPRESENTATION_ITEM('')
);
#250=(
BOUNDED_CURVE()
B_SPLINE_CURVE(5,(#15490,#15491,#15492,#15493,#15494,#15495),
 .UNSPECIFIED.,.F.,.F.)
B_SPLINE_CURVE_WITH_KNOTS((6,6),(0.984324037881406,1.),.UNSPECIFIED.)
CURVE()
GEOMETRIC_REPRESENTATION_ITEM()
RATIONAL_B_SPLINE_CURVE((1.,1.,1.,1.,1.,1.))
REPRESENTATION_ITEM('')
);
#251=(
BOUNDED_CURVE()
B_SPLINE_CURVE(5,(#15607,#15608,#15609,#15610,#15611,#15612),
 .UNSPECIFIED.,.F.,.F.)
B_SPLINE_CURVE_WITH_KNOTS((6,6),(0.984324037881406,1.),.UNSPECIFIED.)
CURVE()
GEOMETRIC_REPRESENTATION_ITEM()
RATIONAL_B_SPLINE_CURVE((1.,1.,1.,1.,1.,1.))
REPRESENTATION_ITEM('')
);
#252=(
BOUNDED_CURVE()
B_SPLINE_CURVE(5,(#15724,#15725,#15726,#15727,#15728,#15729),
 .UNSPECIFIED.,.F.,.F.)
B_SPLINE_CURVE_WITH_KNOTS((6,6),(0.984324037881405,1.),.UNSPECIFIED.)
CURVE()
GEOMETRIC_REPRESENTATION_ITEM()
RATIONAL_B_SPLINE_CURVE((1.,1.,1.,1.,1.,1.))
REPRESENTATION_ITEM('')
);
#253=(
BOUNDED_CURVE()
B_SPLINE_CURVE(5,(#15779,#15780,#15781,#15782,#15783,#15784),
 .UNSPECIFIED.,.F.,.F.)
B_SPLINE_CURVE_WITH_KNOTS((6,6),(0.984324037881406,1.),.UNSPECIFIED.)
CURVE()
GEOMETRIC_REPRESENTATION_ITEM()
RATIONAL_B_SPLINE_CURVE((1.,1.,1.,1.,1.,1.))
REPRESENTATION_ITEM('')
);
#254=(
BOUNDED_CURVE()
B_SPLINE_CURVE(5,(#15834,#15835,#15836,#15837,#15838,#15839),
 .UNSPECIFIED.,.F.,.F.)
B_SPLINE_CURVE_WITH_KNOTS((6,6),(0.984324037881405,1.),.UNSPECIFIED.)
CURVE()
GEOMETRIC_REPRESENTATION_ITEM()
RATIONAL_B_SPLINE_CURVE((1.,1.,1.,1.,1.,1.))
REPRESENTATION_ITEM('')
);
#255=(
BOUNDED_CURVE()
B_SPLINE_CURVE(5,(#16035,#16036,#16037,#16038,#16039,#16040,#16041,#16042,
#16043,#16044,#16045,#16046,#16047,#16048,#16049,#16050,#16051,#16052,#16053,
#16054,#16055,#16056,#16057,#16058,#16059,#16060,#16061,#16062,#16063,#16064,
#16065,#16066,#16067,#16068,#16069),.UNSPECIFIED.,.F.,.F.)
B_SPLINE_CURVE_WITH_KNOTS((6,1,1,1,1,1,1,1,1,1,1,1,1,1,1,1,1,1,1,1,1,1,
1,1,1,1,1,1,1,1,6),(0.,0.0333333333333333,0.0666666666666667,0.1,0.133333333333333,
0.166666666666667,0.2,0.233333333333333,0.266666666666667,0.3,0.333333333333333,
0.366666666666667,0.4,0.433333333333333,0.466666666666667,0.5,0.533333333333333,
0.566666666666667,0.6,0.633333333333333,0.666666666666667,0.7,0.733333333333333,
0.766666666666667,0.8,0.833333333333333,0.866666666666667,0.9,0.933333333333333,
0.966666666666667,1.),.UNSPECIFIED.)
CURVE()
GEOMETRIC_REPRESENTATION_ITEM()
RATIONAL_B_SPLINE_CURVE((1.,1.,1.,1.,1.,1.,1.,1.,1.,1.,1.,1.,1.,1.,1.,1.,
1.,1.,1.,1.,1.,1.,1.,1.,1.,1.,1.,1.,1.,1.,1.,1.,1.,1.,1.))
REPRESENTATION_ITEM('')
);
#256=(
BOUNDED_CURVE()
B_SPLINE_CURVE(5,(#16071,#16072,#16073,#16074,#16075,#16076,#16077,#16078,
#16079,#16080,#16081,#16082,#16083,#16084,#16085,#16086,#16087,#16088,#16089,
#16090,#16091,#16092,#16093,#16094,#16095,#16096,#16097,#16098,#16099,#16100,
#16101,#16102,#16103,#16104,#16105),.UNSPECIFIED.,.F.,.F.)
B_SPLINE_CURVE_WITH_KNOTS((6,1,1,1,1,1,1,1,1,1,1,1,1,1,1,1,1,1,1,1,1,1,
1,1,1,1,1,1,1,1,6),(0.,0.0333333333333333,0.0666666666666667,0.1,0.133333333333333,
0.166666666666667,0.2,0.233333333333333,0.266666666666667,0.3,0.333333333333333,
0.366666666666667,0.4,0.433333333333333,0.466666666666667,0.5,0.533333333333333,
0.566666666666667,0.6,0.633333333333333,0.666666666666667,0.7,0.733333333333333,
0.766666666666667,0.8,0.833333333333333,0.866666666666667,0.9,0.933333333333333,
0.966666666666667,1.),.UNSPECIFIED.)
CURVE()
GEOMETRIC_REPRESENTATION_ITEM()
RATIONAL_B_SPLINE_CURVE((1.,1.,1.,1.,1.,1.,1.,1.,1.,1.,1.,1.,1.,1.,1.,1.,
1.,1.,1.,1.,1.,1.,1.,1.,1.,1.,1.,1.,1.,1.,1.,1.,1.,1.,1.))
REPRESENTATION_ITEM('')
);
#257=(
BOUNDED_CURVE()
B_SPLINE_CURVE(5,(#16109,#16110,#16111,#16112,#16113,#16114,#16115,#16116,
#16117,#16118,#16119,#16120,#16121,#16122,#16123,#16124,#16125,#16126,#16127,
#16128,#16129,#16130,#16131,#16132,#16133,#16134,#16135,#16136,#16137,#16138,
#16139,#16140,#16141,#16142,#16143),.UNSPECIFIED.,.F.,.F.)
B_SPLINE_CURVE_WITH_KNOTS((6,1,1,1,1,1,1,1,1,1,1,1,1,1,1,1,1,1,1,1,1,1,
1,1,1,1,1,1,1,1,6),(0.,0.0333333333333333,0.0666666666666667,0.1,0.133333333333333,
0.166666666666667,0.2,0.233333333333333,0.266666666666667,0.3,0.333333333333333,
0.366666666666667,0.4,0.433333333333333,0.466666666666667,0.5,0.533333333333333,
0.566666666666667,0.6,0.633333333333333,0.666666666666667,0.7,0.733333333333333,
0.766666666666667,0.8,0.833333333333333,0.866666666666667,0.9,0.933333333333333,
0.966666666666667,1.),.UNSPECIFIED.)
CURVE()
GEOMETRIC_REPRESENTATION_ITEM()
RATIONAL_B_SPLINE_CURVE((1.,1.,1.,1.,1.,1.,1.,1.,1.,1.,1.,1.,1.,1.,1.,1.,
1.,1.,1.,1.,1.,1.,1.,1.,1.,1.,1.,1.,1.,1.,1.,1.,1.,1.,1.))
REPRESENTATION_ITEM('')
);
#258=(
BOUNDED_CURVE()
B_SPLINE_CURVE(5,(#16145,#16146,#16147,#16148,#16149,#16150,#16151,#16152,
#16153,#16154,#16155,#16156,#16157,#16158,#16159,#16160,#16161,#16162,#16163,
#16164,#16165,#16166,#16167,#16168,#16169,#16170,#16171,#16172,#16173,#16174,
#16175,#16176,#16177,#16178,#16179),.UNSPECIFIED.,.F.,.F.)
B_SPLINE_CURVE_WITH_KNOTS((6,1,1,1,1,1,1,1,1,1,1,1,1,1,1,1,1,1,1,1,1,1,
1,1,1,1,1,1,1,1,6),(0.,0.0333333333333333,0.0666666666666667,0.1,0.133333333333333,
0.166666666666667,0.2,0.233333333333333,0.266666666666667,0.3,0.333333333333333,
0.366666666666667,0.4,0.433333333333333,0.466666666666667,0.5,0.533333333333333,
0.566666666666667,0.6,0.633333333333333,0.666666666666667,0.7,0.733333333333333,
0.766666666666667,0.8,0.833333333333333,0.866666666666667,0.9,0.933333333333333,
0.966666666666667,1.),.UNSPECIFIED.)
CURVE()
GEOMETRIC_REPRESENTATION_ITEM()
RATIONAL_B_SPLINE_CURVE((1.,1.,1.,1.,1.,1.,1.,1.,1.,1.,1.,1.,1.,1.,1.,1.,
1.,1.,1.,1.,1.,1.,1.,1.,1.,1.,1.,1.,1.,1.,1.,1.,1.,1.,1.))
REPRESENTATION_ITEM('')
);
#259=(
BOUNDED_CURVE()
B_SPLINE_CURVE(5,(#16183,#16184,#16185,#16186,#16187,#16188,#16189,#16190,
#16191,#16192,#16193,#16194,#16195,#16196,#16197,#16198,#16199,#16200,#16201,
#16202,#16203,#16204,#16205,#16206,#16207,#16208,#16209,#16210,#16211,#16212,
#16213,#16214,#16215,#16216,#16217),.UNSPECIFIED.,.F.,.F.)
B_SPLINE_CURVE_WITH_KNOTS((6,1,1,1,1,1,1,1,1,1,1,1,1,1,1,1,1,1,1,1,1,1,
1,1,1,1,1,1,1,1,6),(0.,0.0333333333333333,0.0666666666666667,0.1,0.133333333333333,
0.166666666666667,0.2,0.233333333333333,0.266666666666667,0.3,0.333333333333333,
0.366666666666667,0.4,0.433333333333333,0.466666666666667,0.5,0.533333333333333,
0.566666666666667,0.6,0.633333333333333,0.666666666666667,0.7,0.733333333333333,
0.766666666666667,0.8,0.833333333333333,0.866666666666667,0.9,0.933333333333333,
0.966666666666667,1.),.UNSPECIFIED.)
CURVE()
GEOMETRIC_REPRESENTATION_ITEM()
RATIONAL_B_SPLINE_CURVE((1.,1.,1.,1.,1.,1.,1.,1.,1.,1.,1.,1.,1.,1.,1.,1.,
1.,1.,1.,1.,1.,1.,1.,1.,1.,1.,1.,1.,1.,1.,1.,1.,1.,1.,1.))
REPRESENTATION_ITEM('')
);
#260=(
BOUNDED_CURVE()
B_SPLINE_CURVE(5,(#16219,#16220,#16221,#16222,#16223,#16224,#16225,#16226,
#16227,#16228,#16229,#16230,#16231,#16232,#16233,#16234,#16235,#16236,#16237,
#16238,#16239,#16240,#16241,#16242,#16243,#16244,#16245,#16246,#16247,#16248,
#16249,#16250,#16251,#16252,#16253),.UNSPECIFIED.,.F.,.F.)
B_SPLINE_CURVE_WITH_KNOTS((6,1,1,1,1,1,1,1,1,1,1,1,1,1,1,1,1,1,1,1,1,1,
1,1,1,1,1,1,1,1,6),(0.,0.0333333333333333,0.0666666666666667,0.1,0.133333333333333,
0.166666666666667,0.2,0.233333333333333,0.266666666666667,0.3,0.333333333333333,
0.366666666666667,0.4,0.433333333333333,0.466666666666667,0.5,0.533333333333333,
0.566666666666667,0.6,0.633333333333333,0.666666666666667,0.7,0.733333333333333,
0.766666666666667,0.8,0.833333333333333,0.866666666666667,0.9,0.933333333333333,
0.966666666666667,1.),.UNSPECIFIED.)
CURVE()
GEOMETRIC_REPRESENTATION_ITEM()
RATIONAL_B_SPLINE_CURVE((1.,1.,1.,1.,1.,1.,1.,1.,1.,1.,1.,1.,1.,1.,1.,1.,
1.,1.,1.,1.,1.,1.,1.,1.,1.,1.,1.,1.,1.,1.,1.,1.,1.,1.,1.))
REPRESENTATION_ITEM('')
);
#261=(
BOUNDED_CURVE()
B_SPLINE_CURVE(5,(#16257,#16258,#16259,#16260,#16261,#16262,#16263,#16264,
#16265,#16266,#16267,#16268,#16269,#16270,#16271,#16272,#16273,#16274,#16275,
#16276,#16277,#16278,#16279,#16280,#16281,#16282,#16283,#16284,#16285,#16286,
#16287,#16288,#16289,#16290,#16291),.UNSPECIFIED.,.F.,.F.)
B_SPLINE_CURVE_WITH_KNOTS((6,1,1,1,1,1,1,1,1,1,1,1,1,1,1,1,1,1,1,1,1,1,
1,1,1,1,1,1,1,1,6),(0.,0.0333333333333333,0.0666666666666667,0.1,0.133333333333333,
0.166666666666667,0.2,0.233333333333333,0.266666666666667,0.3,0.333333333333333,
0.366666666666667,0.4,0.433333333333333,0.466666666666667,0.5,0.533333333333333,
0.566666666666667,0.6,0.633333333333333,0.666666666666667,0.7,0.733333333333333,
0.766666666666667,0.8,0.833333333333333,0.866666666666667,0.9,0.933333333333333,
0.966666666666667,1.),.UNSPECIFIED.)
CURVE()
GEOMETRIC_REPRESENTATION_ITEM()
RATIONAL_B_SPLINE_CURVE((1.,1.,1.,1.,1.,1.,1.,1.,1.,1.,1.,1.,1.,1.,1.,1.,
1.,1.,1.,1.,1.,1.,1.,1.,1.,1.,1.,1.,1.,1.,1.,1.,1.,1.,1.))
REPRESENTATION_ITEM('')
);
#262=(
BOUNDED_CURVE()
B_SPLINE_CURVE(5,(#16293,#16294,#16295,#16296,#16297,#16298,#16299,#16300,
#16301,#16302,#16303,#16304,#16305,#16306,#16307,#16308,#16309,#16310,#16311,
#16312,#16313,#16314,#16315,#16316,#16317,#16318,#16319,#16320,#16321,#16322,
#16323,#16324,#16325,#16326,#16327),.UNSPECIFIED.,.F.,.F.)
B_SPLINE_CURVE_WITH_KNOTS((6,1,1,1,1,1,1,1,1,1,1,1,1,1,1,1,1,1,1,1,1,1,
1,1,1,1,1,1,1,1,6),(0.,0.0333333333333333,0.0666666666666667,0.1,0.133333333333333,
0.166666666666667,0.2,0.233333333333333,0.266666666666667,0.3,0.333333333333333,
0.366666666666667,0.4,0.433333333333333,0.466666666666667,0.5,0.533333333333333,
0.566666666666667,0.6,0.633333333333333,0.666666666666667,0.7,0.733333333333333,
0.766666666666667,0.8,0.833333333333333,0.866666666666667,0.9,0.933333333333333,
0.966666666666667,1.),.UNSPECIFIED.)
CURVE()
GEOMETRIC_REPRESENTATION_ITEM()
RATIONAL_B_SPLINE_CURVE((1.,1.,1.,1.,1.,1.,1.,1.,1.,1.,1.,1.,1.,1.,1.,1.,
1.,1.,1.,1.,1.,1.,1.,1.,1.,1.,1.,1.,1.,1.,1.,1.,1.,1.,1.))
REPRESENTATION_ITEM('')
);
#263=(
BOUNDED_CURVE()
B_SPLINE_CURVE(5,(#16331,#16332,#16333,#16334,#16335,#16336,#16337,#16338,
#16339,#16340,#16341,#16342,#16343,#16344,#16345,#16346,#16347,#16348,#16349,
#16350,#16351,#16352,#16353,#16354,#16355,#16356,#16357,#16358,#16359,#16360,
#16361,#16362,#16363,#16364,#16365),.UNSPECIFIED.,.F.,.F.)
B_SPLINE_CURVE_WITH_KNOTS((6,1,1,1,1,1,1,1,1,1,1,1,1,1,1,1,1,1,1,1,1,1,
1,1,1,1,1,1,1,1,6),(0.,0.0333333333333333,0.0666666666666667,0.1,0.133333333333333,
0.166666666666667,0.2,0.233333333333333,0.266666666666667,0.3,0.333333333333333,
0.366666666666667,0.4,0.433333333333333,0.466666666666667,0.5,0.533333333333333,
0.566666666666667,0.6,0.633333333333333,0.666666666666667,0.7,0.733333333333333,
0.766666666666667,0.8,0.833333333333333,0.866666666666667,0.9,0.933333333333333,
0.966666666666667,1.),.UNSPECIFIED.)
CURVE()
GEOMETRIC_REPRESENTATION_ITEM()
RATIONAL_B_SPLINE_CURVE((1.,1.,1.,1.,1.,1.,1.,1.,1.,1.,1.,1.,1.,1.,1.,1.,
1.,1.,1.,1.,1.,1.,1.,1.,1.,1.,1.,1.,1.,1.,1.,1.,1.,1.,1.))
REPRESENTATION_ITEM('')
);
#264=(
BOUNDED_CURVE()
B_SPLINE_CURVE(5,(#16367,#16368,#16369,#16370,#16371,#16372,#16373,#16374,
#16375,#16376,#16377,#16378,#16379,#16380,#16381,#16382,#16383,#16384,#16385,
#16386,#16387,#16388,#16389,#16390,#16391,#16392,#16393,#16394,#16395,#16396,
#16397,#16398,#16399,#16400,#16401),.UNSPECIFIED.,.F.,.F.)
B_SPLINE_CURVE_WITH_KNOTS((6,1,1,1,1,1,1,1,1,1,1,1,1,1,1,1,1,1,1,1,1,1,
1,1,1,1,1,1,1,1,6),(0.,0.0333333333333333,0.0666666666666667,0.1,0.133333333333333,
0.166666666666667,0.2,0.233333333333333,0.266666666666667,0.3,0.333333333333333,
0.366666666666667,0.4,0.433333333333333,0.466666666666667,0.5,0.533333333333333,
0.566666666666667,0.6,0.633333333333333,0.666666666666667,0.7,0.733333333333333,
0.766666666666667,0.8,0.833333333333333,0.866666666666667,0.9,0.933333333333333,
0.966666666666667,1.),.UNSPECIFIED.)
CURVE()
GEOMETRIC_REPRESENTATION_ITEM()
RATIONAL_B_SPLINE_CURVE((1.,1.,1.,1.,1.,1.,1.,1.,1.,1.,1.,1.,1.,1.,1.,1.,
1.,1.,1.,1.,1.,1.,1.,1.,1.,1.,1.,1.,1.,1.,1.,1.,1.,1.,1.))
REPRESENTATION_ITEM('')
);
#265=(
BOUNDED_CURVE()
B_SPLINE_CURVE(5,(#16405,#16406,#16407,#16408,#16409,#16410,#16411,#16412,
#16413,#16414,#16415,#16416,#16417,#16418,#16419,#16420,#16421,#16422,#16423,
#16424,#16425,#16426,#16427,#16428,#16429,#16430,#16431,#16432,#16433,#16434,
#16435,#16436,#16437,#16438,#16439),.UNSPECIFIED.,.F.,.F.)
B_SPLINE_CURVE_WITH_KNOTS((6,1,1,1,1,1,1,1,1,1,1,1,1,1,1,1,1,1,1,1,1,1,
1,1,1,1,1,1,1,1,6),(0.,0.0333333333333333,0.0666666666666667,0.1,0.133333333333333,
0.166666666666667,0.2,0.233333333333333,0.266666666666667,0.3,0.333333333333333,
0.366666666666667,0.4,0.433333333333333,0.466666666666667,0.5,0.533333333333333,
0.566666666666667,0.6,0.633333333333333,0.666666666666667,0.7,0.733333333333333,
0.766666666666667,0.8,0.833333333333333,0.866666666666667,0.9,0.933333333333333,
0.966666666666667,1.),.UNSPECIFIED.)
CURVE()
GEOMETRIC_REPRESENTATION_ITEM()
RATIONAL_B_SPLINE_CURVE((1.,1.,1.,1.,1.,1.,1.,1.,1.,1.,1.,1.,1.,1.,1.,1.,
1.,1.,1.,1.,1.,1.,1.,1.,1.,1.,1.,1.,1.,1.,1.,1.,1.,1.,1.))
REPRESENTATION_ITEM('')
);
#266=(
BOUNDED_CURVE()
B_SPLINE_CURVE(5,(#16441,#16442,#16443,#16444,#16445,#16446,#16447,#16448,
#16449,#16450,#16451,#16452,#16453,#16454,#16455,#16456,#16457,#16458,#16459,
#16460,#16461,#16462,#16463,#16464,#16465,#16466,#16467,#16468,#16469,#16470,
#16471,#16472,#16473,#16474,#16475),.UNSPECIFIED.,.F.,.F.)
B_SPLINE_CURVE_WITH_KNOTS((6,1,1,1,1,1,1,1,1,1,1,1,1,1,1,1,1,1,1,1,1,1,
1,1,1,1,1,1,1,1,6),(0.,0.0333333333333333,0.0666666666666667,0.1,0.133333333333333,
0.166666666666667,0.2,0.233333333333333,0.266666666666667,0.3,0.333333333333333,
0.366666666666667,0.4,0.433333333333333,0.466666666666667,0.5,0.533333333333333,
0.566666666666667,0.6,0.633333333333333,0.666666666666667,0.7,0.733333333333333,
0.766666666666667,0.8,0.833333333333333,0.866666666666667,0.9,0.933333333333333,
0.966666666666667,1.),.UNSPECIFIED.)
CURVE()
GEOMETRIC_REPRESENTATION_ITEM()
RATIONAL_B_SPLINE_CURVE((1.,1.,1.,1.,1.,1.,1.,1.,1.,1.,1.,1.,1.,1.,1.,1.,
1.,1.,1.,1.,1.,1.,1.,1.,1.,1.,1.,1.,1.,1.,1.,1.,1.,1.,1.))
REPRESENTATION_ITEM('')
);
#267=(
BOUNDED_CURVE()
B_SPLINE_CURVE(5,(#16479,#16480,#16481,#16482,#16483,#16484,#16485,#16486,
#16487,#16488,#16489,#16490,#16491,#16492,#16493,#16494,#16495,#16496,#16497,
#16498,#16499,#16500,#16501,#16502,#16503,#16504,#16505,#16506,#16507,#16508,
#16509,#16510,#16511,#16512,#16513),.UNSPECIFIED.,.F.,.F.)
B_SPLINE_CURVE_WITH_KNOTS((6,1,1,1,1,1,1,1,1,1,1,1,1,1,1,1,1,1,1,1,1,1,
1,1,1,1,1,1,1,1,6),(0.,0.0333333333333333,0.0666666666666667,0.1,0.133333333333333,
0.166666666666667,0.2,0.233333333333333,0.266666666666667,0.3,0.333333333333333,
0.366666666666667,0.4,0.433333333333333,0.466666666666667,0.5,0.533333333333333,
0.566666666666667,0.6,0.633333333333333,0.666666666666667,0.7,0.733333333333333,
0.766666666666667,0.8,0.833333333333333,0.866666666666667,0.9,0.933333333333333,
0.966666666666667,1.),.UNSPECIFIED.)
CURVE()
GEOMETRIC_REPRESENTATION_ITEM()
RATIONAL_B_SPLINE_CURVE((1.,1.,1.,1.,1.,1.,1.,1.,1.,1.,1.,1.,1.,1.,1.,1.,
1.,1.,1.,1.,1.,1.,1.,1.,1.,1.,1.,1.,1.,1.,1.,1.,1.,1.,1.))
REPRESENTATION_ITEM('')
);
#268=(
BOUNDED_CURVE()
B_SPLINE_CURVE(5,(#16515,#16516,#16517,#16518,#16519,#16520,#16521,#16522,
#16523,#16524,#16525,#16526,#16527,#16528,#16529,#16530,#16531,#16532,#16533,
#16534,#16535,#16536,#16537,#16538,#16539,#16540,#16541,#16542,#16543,#16544,
#16545,#16546,#16547,#16548,#16549),.UNSPECIFIED.,.F.,.F.)
B_SPLINE_CURVE_WITH_KNOTS((6,1,1,1,1,1,1,1,1,1,1,1,1,1,1,1,1,1,1,1,1,1,
1,1,1,1,1,1,1,1,6),(0.,0.0333333333333333,0.0666666666666667,0.1,0.133333333333333,
0.166666666666667,0.2,0.233333333333333,0.266666666666667,0.3,0.333333333333333,
0.366666666666667,0.4,0.433333333333333,0.466666666666667,0.5,0.533333333333333,
0.566666666666667,0.6,0.633333333333333,0.666666666666667,0.7,0.733333333333333,
0.766666666666667,0.8,0.833333333333333,0.866666666666667,0.9,0.933333333333333,
0.966666666666667,1.),.UNSPECIFIED.)
CURVE()
GEOMETRIC_REPRESENTATION_ITEM()
RATIONAL_B_SPLINE_CURVE((1.,1.,1.,1.,1.,1.,1.,1.,1.,1.,1.,1.,1.,1.,1.,1.,
1.,1.,1.,1.,1.,1.,1.,1.,1.,1.,1.,1.,1.,1.,1.,1.,1.,1.,1.))
REPRESENTATION_ITEM('')
);
#269=(
BOUNDED_CURVE()
B_SPLINE_CURVE(5,(#16553,#16554,#16555,#16556,#16557,#16558,#16559,#16560,
#16561,#16562,#16563,#16564,#16565,#16566,#16567,#16568,#16569,#16570,#16571,
#16572,#16573,#16574,#16575,#16576,#16577,#16578,#16579,#16580,#16581,#16582,
#16583,#16584,#16585,#16586,#16587),.UNSPECIFIED.,.F.,.F.)
B_SPLINE_CURVE_WITH_KNOTS((6,1,1,1,1,1,1,1,1,1,1,1,1,1,1,1,1,1,1,1,1,1,
1,1,1,1,1,1,1,1,6),(0.,0.0333333333333333,0.0666666666666667,0.1,0.133333333333333,
0.166666666666667,0.2,0.233333333333333,0.266666666666667,0.3,0.333333333333333,
0.366666666666667,0.4,0.433333333333333,0.466666666666667,0.5,0.533333333333333,
0.566666666666667,0.6,0.633333333333333,0.666666666666667,0.7,0.733333333333333,
0.766666666666667,0.8,0.833333333333333,0.866666666666667,0.9,0.933333333333333,
0.966666666666667,1.),.UNSPECIFIED.)
CURVE()
GEOMETRIC_REPRESENTATION_ITEM()
RATIONAL_B_SPLINE_CURVE((1.,1.,1.,1.,1.,1.,1.,1.,1.,1.,1.,1.,1.,1.,1.,1.,
1.,1.,1.,1.,1.,1.,1.,1.,1.,1.,1.,1.,1.,1.,1.,1.,1.,1.,1.))
REPRESENTATION_ITEM('')
);
#270=(
BOUNDED_CURVE()
B_SPLINE_CURVE(5,(#16589,#16590,#16591,#16592,#16593,#16594,#16595,#16596,
#16597,#16598,#16599,#16600,#16601,#16602,#16603,#16604,#16605,#16606,#16607,
#16608,#16609,#16610,#16611,#16612,#16613,#16614,#16615,#16616,#16617,#16618,
#16619,#16620,#16621,#16622,#16623),.UNSPECIFIED.,.F.,.F.)
B_SPLINE_CURVE_WITH_KNOTS((6,1,1,1,1,1,1,1,1,1,1,1,1,1,1,1,1,1,1,1,1,1,
1,1,1,1,1,1,1,1,6),(0.,0.0333333333333333,0.0666666666666667,0.1,0.133333333333333,
0.166666666666667,0.2,0.233333333333333,0.266666666666667,0.3,0.333333333333333,
0.366666666666667,0.4,0.433333333333333,0.466666666666667,0.5,0.533333333333333,
0.566666666666667,0.6,0.633333333333333,0.666666666666667,0.7,0.733333333333333,
0.766666666666667,0.8,0.833333333333333,0.866666666666667,0.9,0.933333333333333,
0.966666666666667,1.),.UNSPECIFIED.)
CURVE()
GEOMETRIC_REPRESENTATION_ITEM()
RATIONAL_B_SPLINE_CURVE((1.,1.,1.,1.,1.,1.,1.,1.,1.,1.,1.,1.,1.,1.,1.,1.,
1.,1.,1.,1.,1.,1.,1.,1.,1.,1.,1.,1.,1.,1.,1.,1.,1.,1.,1.))
REPRESENTATION_ITEM('')
);
#271=(
BOUNDED_CURVE()
B_SPLINE_CURVE(5,(#16627,#16628,#16629,#16630,#16631,#16632,#16633,#16634,
#16635,#16636,#16637,#16638,#16639,#16640,#16641,#16642,#16643,#16644,#16645,
#16646,#16647,#16648,#16649,#16650,#16651,#16652,#16653,#16654,#16655,#16656,
#16657,#16658,#16659,#16660,#16661),.UNSPECIFIED.,.F.,.F.)
B_SPLINE_CURVE_WITH_KNOTS((6,1,1,1,1,1,1,1,1,1,1,1,1,1,1,1,1,1,1,1,1,1,
1,1,1,1,1,1,1,1,6),(0.,0.0333333333333333,0.0666666666666667,0.1,0.133333333333333,
0.166666666666667,0.2,0.233333333333333,0.266666666666667,0.3,0.333333333333333,
0.366666666666667,0.4,0.433333333333333,0.466666666666667,0.5,0.533333333333333,
0.566666666666667,0.6,0.633333333333333,0.666666666666667,0.7,0.733333333333333,
0.766666666666667,0.8,0.833333333333333,0.866666666666667,0.9,0.933333333333333,
0.966666666666667,1.),.UNSPECIFIED.)
CURVE()
GEOMETRIC_REPRESENTATION_ITEM()
RATIONAL_B_SPLINE_CURVE((1.,1.,1.,1.,1.,1.,1.,1.,1.,1.,1.,1.,1.,1.,1.,1.,
1.,1.,1.,1.,1.,1.,1.,1.,1.,1.,1.,1.,1.,1.,1.,1.,1.,1.,1.))
REPRESENTATION_ITEM('')
);
#272=(
BOUNDED_CURVE()
B_SPLINE_CURVE(5,(#16663,#16664,#16665,#16666,#16667,#16668,#16669,#16670,
#16671,#16672,#16673,#16674,#16675,#16676,#16677,#16678,#16679,#16680,#16681,
#16682,#16683,#16684,#16685,#16686,#16687,#16688,#16689,#16690,#16691,#16692,
#16693,#16694,#16695,#16696,#16697),.UNSPECIFIED.,.F.,.F.)
B_SPLINE_CURVE_WITH_KNOTS((6,1,1,1,1,1,1,1,1,1,1,1,1,1,1,1,1,1,1,1,1,1,
1,1,1,1,1,1,1,1,6),(0.,0.0333333333333333,0.0666666666666667,0.1,0.133333333333333,
0.166666666666667,0.2,0.233333333333333,0.266666666666667,0.3,0.333333333333333,
0.366666666666667,0.4,0.433333333333333,0.466666666666667,0.5,0.533333333333333,
0.566666666666667,0.6,0.633333333333333,0.666666666666667,0.7,0.733333333333333,
0.766666666666667,0.8,0.833333333333333,0.866666666666667,0.9,0.933333333333333,
0.966666666666667,1.),.UNSPECIFIED.)
CURVE()
GEOMETRIC_REPRESENTATION_ITEM()
RATIONAL_B_SPLINE_CURVE((1.,1.,1.,1.,1.,1.,1.,1.,1.,1.,1.,1.,1.,1.,1.,1.,
1.,1.,1.,1.,1.,1.,1.,1.,1.,1.,1.,1.,1.,1.,1.,1.,1.,1.,1.))
REPRESENTATION_ITEM('')
);
#273=(
BOUNDED_CURVE()
B_SPLINE_CURVE(5,(#16701,#16702,#16703,#16704,#16705,#16706,#16707,#16708,
#16709,#16710,#16711,#16712,#16713,#16714,#16715,#16716,#16717,#16718,#16719,
#16720,#16721,#16722,#16723,#16724,#16725,#16726,#16727,#16728,#16729,#16730,
#16731,#16732,#16733,#16734,#16735),.UNSPECIFIED.,.F.,.F.)
B_SPLINE_CURVE_WITH_KNOTS((6,1,1,1,1,1,1,1,1,1,1,1,1,1,1,1,1,1,1,1,1,1,
1,1,1,1,1,1,1,1,6),(0.,0.0333333333333333,0.0666666666666667,0.1,0.133333333333333,
0.166666666666667,0.2,0.233333333333333,0.266666666666667,0.3,0.333333333333333,
0.366666666666667,0.4,0.433333333333333,0.466666666666667,0.5,0.533333333333333,
0.566666666666667,0.6,0.633333333333333,0.666666666666667,0.7,0.733333333333333,
0.766666666666667,0.8,0.833333333333333,0.866666666666667,0.9,0.933333333333333,
0.966666666666667,1.),.UNSPECIFIED.)
CURVE()
GEOMETRIC_REPRESENTATION_ITEM()
RATIONAL_B_SPLINE_CURVE((1.,1.,1.,1.,1.,1.,1.,1.,1.,1.,1.,1.,1.,1.,1.,1.,
1.,1.,1.,1.,1.,1.,1.,1.,1.,1.,1.,1.,1.,1.,1.,1.,1.,1.,1.))
REPRESENTATION_ITEM('')
);
#274=(
BOUNDED_CURVE()
B_SPLINE_CURVE(5,(#16737,#16738,#16739,#16740,#16741,#16742,#16743,#16744,
#16745,#16746,#16747,#16748,#16749,#16750,#16751,#16752,#16753,#16754,#16755,
#16756,#16757,#16758,#16759,#16760,#16761,#16762,#16763,#16764,#16765,#16766,
#16767,#16768,#16769,#16770,#16771),.UNSPECIFIED.,.F.,.F.)
B_SPLINE_CURVE_WITH_KNOTS((6,1,1,1,1,1,1,1,1,1,1,1,1,1,1,1,1,1,1,1,1,1,
1,1,1,1,1,1,1,1,6),(0.,0.0333333333333333,0.0666666666666667,0.1,0.133333333333333,
0.166666666666667,0.2,0.233333333333333,0.266666666666667,0.3,0.333333333333333,
0.366666666666667,0.4,0.433333333333333,0.466666666666667,0.5,0.533333333333333,
0.566666666666667,0.6,0.633333333333333,0.666666666666667,0.7,0.733333333333333,
0.766666666666667,0.8,0.833333333333333,0.866666666666667,0.9,0.933333333333333,
0.966666666666667,1.),.UNSPECIFIED.)
CURVE()
GEOMETRIC_REPRESENTATION_ITEM()
RATIONAL_B_SPLINE_CURVE((1.,1.,1.,1.,1.,1.,1.,1.,1.,1.,1.,1.,1.,1.,1.,1.,
1.,1.,1.,1.,1.,1.,1.,1.,1.,1.,1.,1.,1.,1.,1.,1.,1.,1.,1.))
REPRESENTATION_ITEM('')
);
#275=(
BOUNDED_CURVE()
B_SPLINE_CURVE(5,(#16775,#16776,#16777,#16778,#16779,#16780,#16781,#16782,
#16783,#16784,#16785,#16786,#16787,#16788,#16789,#16790,#16791,#16792,#16793,
#16794,#16795,#16796,#16797,#16798,#16799,#16800,#16801,#16802,#16803,#16804,
#16805,#16806,#16807,#16808,#16809),.UNSPECIFIED.,.F.,.F.)
B_SPLINE_CURVE_WITH_KNOTS((6,1,1,1,1,1,1,1,1,1,1,1,1,1,1,1,1,1,1,1,1,1,
1,1,1,1,1,1,1,1,6),(0.,0.0333333333333333,0.0666666666666667,0.1,0.133333333333333,
0.166666666666667,0.2,0.233333333333333,0.266666666666667,0.3,0.333333333333333,
0.366666666666667,0.4,0.433333333333333,0.466666666666667,0.5,0.533333333333333,
0.566666666666667,0.6,0.633333333333333,0.666666666666667,0.7,0.733333333333333,
0.766666666666667,0.8,0.833333333333333,0.866666666666667,0.9,0.933333333333333,
0.966666666666667,1.),.UNSPECIFIED.)
CURVE()
GEOMETRIC_REPRESENTATION_ITEM()
RATIONAL_B_SPLINE_CURVE((1.,1.,1.,1.,1.,1.,1.,1.,1.,1.,1.,1.,1.,1.,1.,1.,
1.,1.,1.,1.,1.,1.,1.,1.,1.,1.,1.,1.,1.,1.,1.,1.,1.,1.,1.))
REPRESENTATION_ITEM('')
);
#276=(
BOUNDED_CURVE()
B_SPLINE_CURVE(5,(#16811,#16812,#16813,#16814,#16815,#16816,#16817,#16818,
#16819,#16820,#16821,#16822,#16823,#16824,#16825,#16826,#16827,#16828,#16829,
#16830,#16831,#16832,#16833,#16834,#16835,#16836,#16837,#16838,#16839,#16840,
#16841,#16842,#16843,#16844,#16845),.UNSPECIFIED.,.F.,.F.)
B_SPLINE_CURVE_WITH_KNOTS((6,1,1,1,1,1,1,1,1,1,1,1,1,1,1,1,1,1,1,1,1,1,
1,1,1,1,1,1,1,1,6),(0.,0.0333333333333333,0.0666666666666667,0.1,0.133333333333333,
0.166666666666667,0.2,0.233333333333333,0.266666666666667,0.3,0.333333333333333,
0.366666666666667,0.4,0.433333333333333,0.466666666666667,0.5,0.533333333333333,
0.566666666666667,0.6,0.633333333333333,0.666666666666667,0.7,0.733333333333333,
0.766666666666667,0.8,0.833333333333333,0.866666666666667,0.9,0.933333333333333,
0.966666666666667,1.),.UNSPECIFIED.)
CURVE()
GEOMETRIC_REPRESENTATION_ITEM()
RATIONAL_B_SPLINE_CURVE((1.,1.,1.,1.,1.,1.,1.,1.,1.,1.,1.,1.,1.,1.,1.,1.,
1.,1.,1.,1.,1.,1.,1.,1.,1.,1.,1.,1.,1.,1.,1.,1.,1.,1.,1.))
REPRESENTATION_ITEM('')
);
#277=(
BOUNDED_CURVE()
B_SPLINE_CURVE(5,(#16849,#16850,#16851,#16852,#16853,#16854,#16855,#16856,
#16857,#16858,#16859,#16860,#16861,#16862,#16863,#16864,#16865,#16866,#16867,
#16868,#16869,#16870,#16871,#16872,#16873,#16874,#16875,#16876,#16877,#16878,
#16879,#16880,#16881,#16882,#16883),.UNSPECIFIED.,.F.,.F.)
B_SPLINE_CURVE_WITH_KNOTS((6,1,1,1,1,1,1,1,1,1,1,1,1,1,1,1,1,1,1,1,1,1,
1,1,1,1,1,1,1,1,6),(0.,0.0333333333333333,0.0666666666666667,0.1,0.133333333333333,
0.166666666666667,0.2,0.233333333333333,0.266666666666667,0.3,0.333333333333333,
0.366666666666667,0.4,0.433333333333333,0.466666666666667,0.5,0.533333333333333,
0.566666666666667,0.6,0.633333333333333,0.666666666666667,0.7,0.733333333333333,
0.766666666666667,0.8,0.833333333333333,0.866666666666667,0.9,0.933333333333333,
0.966666666666667,1.),.UNSPECIFIED.)
CURVE()
GEOMETRIC_REPRESENTATION_ITEM()
RATIONAL_B_SPLINE_CURVE((1.,1.,1.,1.,1.,1.,1.,1.,1.,1.,1.,1.,1.,1.,1.,1.,
1.,1.,1.,1.,1.,1.,1.,1.,1.,1.,1.,1.,1.,1.,1.,1.,1.,1.,1.))
REPRESENTATION_ITEM('')
);
#278=(
BOUNDED_CURVE()
B_SPLINE_CURVE(5,(#16885,#16886,#16887,#16888,#16889,#16890,#16891,#16892,
#16893,#16894,#16895,#16896,#16897,#16898,#16899,#16900,#16901,#16902,#16903,
#16904,#16905,#16906,#16907,#16908,#16909,#16910,#16911,#16912,#16913,#16914,
#16915,#16916,#16917,#16918,#16919),.UNSPECIFIED.,.F.,.F.)
B_SPLINE_CURVE_WITH_KNOTS((6,1,1,1,1,1,1,1,1,1,1,1,1,1,1,1,1,1,1,1,1,1,
1,1,1,1,1,1,1,1,6),(0.,0.0333333333333333,0.0666666666666667,0.1,0.133333333333333,
0.166666666666667,0.2,0.233333333333333,0.266666666666667,0.3,0.333333333333333,
0.366666666666667,0.4,0.433333333333333,0.466666666666667,0.5,0.533333333333333,
0.566666666666667,0.6,0.633333333333333,0.666666666666667,0.7,0.733333333333333,
0.766666666666667,0.8,0.833333333333333,0.866666666666667,0.9,0.933333333333333,
0.966666666666667,1.),.UNSPECIFIED.)
CURVE()
GEOMETRIC_REPRESENTATION_ITEM()
RATIONAL_B_SPLINE_CURVE((1.,1.,1.,1.,1.,1.,1.,1.,1.,1.,1.,1.,1.,1.,1.,1.,
1.,1.,1.,1.,1.,1.,1.,1.,1.,1.,1.,1.,1.,1.,1.,1.,1.,1.,1.))
REPRESENTATION_ITEM('')
);
#279=(
BOUNDED_CURVE()
B_SPLINE_CURVE(5,(#16923,#16924,#16925,#16926,#16927,#16928,#16929,#16930,
#16931,#16932,#16933,#16934,#16935,#16936,#16937,#16938,#16939,#16940,#16941,
#16942,#16943,#16944,#16945,#16946,#16947,#16948,#16949,#16950,#16951,#16952,
#16953,#16954,#16955,#16956,#16957),.UNSPECIFIED.,.F.,.F.)
B_SPLINE_CURVE_WITH_KNOTS((6,1,1,1,1,1,1,1,1,1,1,1,1,1,1,1,1,1,1,1,1,1,
1,1,1,1,1,1,1,1,6),(0.,0.0333333333333333,0.0666666666666667,0.1,0.133333333333333,
0.166666666666667,0.2,0.233333333333333,0.266666666666667,0.3,0.333333333333333,
0.366666666666667,0.4,0.433333333333333,0.466666666666667,0.5,0.533333333333333,
0.566666666666667,0.6,0.633333333333333,0.666666666666667,0.7,0.733333333333333,
0.766666666666667,0.8,0.833333333333333,0.866666666666667,0.9,0.933333333333333,
0.966666666666667,1.),.UNSPECIFIED.)
CURVE()
GEOMETRIC_REPRESENTATION_ITEM()
RATIONAL_B_SPLINE_CURVE((1.,1.,1.,1.,1.,1.,1.,1.,1.,1.,1.,1.,1.,1.,1.,1.,
1.,1.,1.,1.,1.,1.,1.,1.,1.,1.,1.,1.,1.,1.,1.,1.,1.,1.,1.))
REPRESENTATION_ITEM('')
);
#280=(
BOUNDED_CURVE()
B_SPLINE_CURVE(5,(#16959,#16960,#16961,#16962,#16963,#16964,#16965,#16966,
#16967,#16968,#16969,#16970,#16971,#16972,#16973,#16974,#16975,#16976,#16977,
#16978,#16979,#16980,#16981,#16982,#16983,#16984,#16985,#16986,#16987,#16988,
#16989,#16990,#16991,#16992,#16993),.UNSPECIFIED.,.F.,.F.)
B_SPLINE_CURVE_WITH_KNOTS((6,1,1,1,1,1,1,1,1,1,1,1,1,1,1,1,1,1,1,1,1,1,
1,1,1,1,1,1,1,1,6),(0.,0.0333333333333333,0.0666666666666667,0.1,0.133333333333333,
0.166666666666667,0.2,0.233333333333333,0.266666666666667,0.3,0.333333333333333,
0.366666666666667,0.4,0.433333333333333,0.466666666666667,0.5,0.533333333333333,
0.566666666666667,0.6,0.633333333333333,0.666666666666667,0.7,0.733333333333333,
0.766666666666667,0.8,0.833333333333333,0.866666666666667,0.9,0.933333333333333,
0.966666666666667,1.),.UNSPECIFIED.)
CURVE()
GEOMETRIC_REPRESENTATION_ITEM()
RATIONAL_B_SPLINE_CURVE((1.,1.,1.,1.,1.,1.,1.,1.,1.,1.,1.,1.,1.,1.,1.,1.,
1.,1.,1.,1.,1.,1.,1.,1.,1.,1.,1.,1.,1.,1.,1.,1.,1.,1.,1.))
REPRESENTATION_ITEM('')
);
#281=(
BOUNDED_CURVE()
B_SPLINE_CURVE(5,(#16997,#16998,#16999,#17000,#17001,#17002,#17003,#17004,
#17005,#17006,#17007,#17008,#17009,#17010,#17011,#17012,#17013,#17014,#17015,
#17016,#17017,#17018,#17019,#17020,#17021,#17022,#17023,#17024,#17025,#17026,
#17027,#17028,#17029,#17030,#17031),.UNSPECIFIED.,.F.,.F.)
B_SPLINE_CURVE_WITH_KNOTS((6,1,1,1,1,1,1,1,1,1,1,1,1,1,1,1,1,1,1,1,1,1,
1,1,1,1,1,1,1,1,6),(0.,0.0333333333333333,0.0666666666666667,0.1,0.133333333333333,
0.166666666666667,0.2,0.233333333333333,0.266666666666667,0.3,0.333333333333333,
0.366666666666667,0.4,0.433333333333333,0.466666666666667,0.5,0.533333333333333,
0.566666666666667,0.6,0.633333333333333,0.666666666666667,0.7,0.733333333333333,
0.766666666666667,0.8,0.833333333333333,0.866666666666667,0.9,0.933333333333333,
0.966666666666667,1.),.UNSPECIFIED.)
CURVE()
GEOMETRIC_REPRESENTATION_ITEM()
RATIONAL_B_SPLINE_CURVE((1.,1.,1.,1.,1.,1.,1.,1.,1.,1.,1.,1.,1.,1.,1.,1.,
1.,1.,1.,1.,1.,1.,1.,1.,1.,1.,1.,1.,1.,1.,1.,1.,1.,1.,1.))
REPRESENTATION_ITEM('')
);
#282=(
BOUNDED_CURVE()
B_SPLINE_CURVE(5,(#17033,#17034,#17035,#17036,#17037,#17038,#17039,#17040,
#17041,#17042,#17043,#17044,#17045,#17046,#17047,#17048,#17049,#17050,#17051,
#17052,#17053,#17054,#17055,#17056,#17057,#17058,#17059,#17060,#17061,#17062,
#17063,#17064,#17065,#17066,#17067),.UNSPECIFIED.,.F.,.F.)
B_SPLINE_CURVE_WITH_KNOTS((6,1,1,1,1,1,1,1,1,1,1,1,1,1,1,1,1,1,1,1,1,1,
1,1,1,1,1,1,1,1,6),(0.,0.0333333333333333,0.0666666666666667,0.1,0.133333333333333,
0.166666666666667,0.2,0.233333333333333,0.266666666666667,0.3,0.333333333333333,
0.366666666666667,0.4,0.433333333333333,0.466666666666667,0.5,0.533333333333333,
0.566666666666667,0.6,0.633333333333333,0.666666666666667,0.7,0.733333333333333,
0.766666666666667,0.8,0.833333333333333,0.866666666666667,0.9,0.933333333333333,
0.966666666666667,1.),.UNSPECIFIED.)
CURVE()
GEOMETRIC_REPRESENTATION_ITEM()
RATIONAL_B_SPLINE_CURVE((1.,1.,1.,1.,1.,1.,1.,1.,1.,1.,1.,1.,1.,1.,1.,1.,
1.,1.,1.,1.,1.,1.,1.,1.,1.,1.,1.,1.,1.,1.,1.,1.,1.,1.,1.))
REPRESENTATION_ITEM('')
);
#283=(
BOUNDED_CURVE()
B_SPLINE_CURVE(5,(#17071,#17072,#17073,#17074,#17075,#17076,#17077,#17078,
#17079,#17080,#17081,#17082,#17083,#17084,#17085,#17086,#17087,#17088,#17089,
#17090,#17091,#17092,#17093,#17094,#17095,#17096,#17097,#17098,#17099,#17100,
#17101,#17102,#17103,#17104,#17105),.UNSPECIFIED.,.F.,.F.)
B_SPLINE_CURVE_WITH_KNOTS((6,1,1,1,1,1,1,1,1,1,1,1,1,1,1,1,1,1,1,1,1,1,
1,1,1,1,1,1,1,1,6),(0.,0.0333333333333333,0.0666666666666667,0.1,0.133333333333333,
0.166666666666667,0.2,0.233333333333333,0.266666666666667,0.3,0.333333333333333,
0.366666666666667,0.4,0.433333333333333,0.466666666666667,0.5,0.533333333333333,
0.566666666666667,0.6,0.633333333333333,0.666666666666667,0.7,0.733333333333333,
0.766666666666667,0.8,0.833333333333333,0.866666666666667,0.9,0.933333333333333,
0.966666666666667,1.),.UNSPECIFIED.)
CURVE()
GEOMETRIC_REPRESENTATION_ITEM()
RATIONAL_B_SPLINE_CURVE((1.,1.,1.,1.,1.,1.,1.,1.,1.,1.,1.,1.,1.,1.,1.,1.,
1.,1.,1.,1.,1.,1.,1.,1.,1.,1.,1.,1.,1.,1.,1.,1.,1.,1.,1.))
REPRESENTATION_ITEM('')
);
#284=(
BOUNDED_CURVE()
B_SPLINE_CURVE(5,(#17107,#17108,#17109,#17110,#17111,#17112,#17113,#17114,
#17115,#17116,#17117,#17118,#17119,#17120,#17121,#17122,#17123,#17124,#17125,
#17126,#17127,#17128,#17129,#17130,#17131,#17132,#17133,#17134,#17135,#17136,
#17137,#17138,#17139,#17140,#17141),.UNSPECIFIED.,.F.,.F.)
B_SPLINE_CURVE_WITH_KNOTS((6,1,1,1,1,1,1,1,1,1,1,1,1,1,1,1,1,1,1,1,1,1,
1,1,1,1,1,1,1,1,6),(0.,0.0333333333333333,0.0666666666666667,0.1,0.133333333333333,
0.166666666666667,0.2,0.233333333333333,0.266666666666667,0.3,0.333333333333333,
0.366666666666667,0.4,0.433333333333333,0.466666666666667,0.5,0.533333333333333,
0.566666666666667,0.6,0.633333333333333,0.666666666666667,0.7,0.733333333333333,
0.766666666666667,0.8,0.833333333333333,0.866666666666667,0.9,0.933333333333333,
0.966666666666667,1.),.UNSPECIFIED.)
CURVE()
GEOMETRIC_REPRESENTATION_ITEM()
RATIONAL_B_SPLINE_CURVE((1.,1.,1.,1.,1.,1.,1.,1.,1.,1.,1.,1.,1.,1.,1.,1.,
1.,1.,1.,1.,1.,1.,1.,1.,1.,1.,1.,1.,1.,1.,1.,1.,1.,1.,1.))
REPRESENTATION_ITEM('')
);
#285=(
BOUNDED_CURVE()
B_SPLINE_CURVE(5,(#17145,#17146,#17147,#17148,#17149,#17150,#17151,#17152,
#17153,#17154,#17155,#17156,#17157,#17158,#17159,#17160,#17161,#17162,#17163,
#17164,#17165,#17166,#17167,#17168,#17169,#17170,#17171,#17172,#17173,#17174,
#17175,#17176,#17177,#17178,#17179),.UNSPECIFIED.,.F.,.F.)
B_SPLINE_CURVE_WITH_KNOTS((6,1,1,1,1,1,1,1,1,1,1,1,1,1,1,1,1,1,1,1,1,1,
1,1,1,1,1,1,1,1,6),(0.,0.0333333333333333,0.0666666666666667,0.1,0.133333333333333,
0.166666666666667,0.2,0.233333333333333,0.266666666666667,0.3,0.333333333333333,
0.366666666666667,0.4,0.433333333333333,0.466666666666667,0.5,0.533333333333333,
0.566666666666667,0.6,0.633333333333333,0.666666666666667,0.7,0.733333333333333,
0.766666666666667,0.8,0.833333333333333,0.866666666666667,0.9,0.933333333333333,
0.966666666666667,1.),.UNSPECIFIED.)
CURVE()
GEOMETRIC_REPRESENTATION_ITEM()
RATIONAL_B_SPLINE_CURVE((1.,1.,1.,1.,1.,1.,1.,1.,1.,1.,1.,1.,1.,1.,1.,1.,
1.,1.,1.,1.,1.,1.,1.,1.,1.,1.,1.,1.,1.,1.,1.,1.,1.,1.,1.))
REPRESENTATION_ITEM('')
);
#286=(
BOUNDED_CURVE()
B_SPLINE_CURVE(5,(#17181,#17182,#17183,#17184,#17185,#17186,#17187,#17188,
#17189,#17190,#17191,#17192,#17193,#17194,#17195,#17196,#17197,#17198,#17199,
#17200,#17201,#17202,#17203,#17204,#17205,#17206,#17207,#17208,#17209,#17210,
#17211,#17212,#17213,#17214,#17215),.UNSPECIFIED.,.F.,.F.)
B_SPLINE_CURVE_WITH_KNOTS((6,1,1,1,1,1,1,1,1,1,1,1,1,1,1,1,1,1,1,1,1,1,
1,1,1,1,1,1,1,1,6),(0.,0.0333333333333333,0.0666666666666667,0.1,0.133333333333333,
0.166666666666667,0.2,0.233333333333333,0.266666666666667,0.3,0.333333333333333,
0.366666666666667,0.4,0.433333333333333,0.466666666666667,0.5,0.533333333333333,
0.566666666666667,0.6,0.633333333333333,0.666666666666667,0.7,0.733333333333333,
0.766666666666667,0.8,0.833333333333333,0.866666666666667,0.9,0.933333333333333,
0.966666666666667,1.),.UNSPECIFIED.)
CURVE()
GEOMETRIC_REPRESENTATION_ITEM()
RATIONAL_B_SPLINE_CURVE((1.,1.,1.,1.,1.,1.,1.,1.,1.,1.,1.,1.,1.,1.,1.,1.,
1.,1.,1.,1.,1.,1.,1.,1.,1.,1.,1.,1.,1.,1.,1.,1.,1.,1.,1.))
REPRESENTATION_ITEM('')
);
#287=(
BOUNDED_CURVE()
B_SPLINE_CURVE(5,(#17219,#17220,#17221,#17222,#17223,#17224,#17225,#17226,
#17227,#17228,#17229,#17230,#17231,#17232,#17233,#17234,#17235,#17236,#17237,
#17238,#17239,#17240,#17241,#17242,#17243,#17244,#17245,#17246,#17247,#17248,
#17249,#17250,#17251,#17252,#17253),.UNSPECIFIED.,.F.,.F.)
B_SPLINE_CURVE_WITH_KNOTS((6,1,1,1,1,1,1,1,1,1,1,1,1,1,1,1,1,1,1,1,1,1,
1,1,1,1,1,1,1,1,6),(0.,0.0333333333333333,0.0666666666666667,0.1,0.133333333333333,
0.166666666666667,0.2,0.233333333333333,0.266666666666667,0.3,0.333333333333333,
0.366666666666667,0.4,0.433333333333333,0.466666666666667,0.5,0.533333333333333,
0.566666666666667,0.6,0.633333333333333,0.666666666666667,0.7,0.733333333333333,
0.766666666666667,0.8,0.833333333333333,0.866666666666667,0.9,0.933333333333333,
0.966666666666667,1.),.UNSPECIFIED.)
CURVE()
GEOMETRIC_REPRESENTATION_ITEM()
RATIONAL_B_SPLINE_CURVE((1.,1.,1.,1.,1.,1.,1.,1.,1.,1.,1.,1.,1.,1.,1.,1.,
1.,1.,1.,1.,1.,1.,1.,1.,1.,1.,1.,1.,1.,1.,1.,1.,1.,1.,1.))
REPRESENTATION_ITEM('')
);
#288=(
BOUNDED_CURVE()
B_SPLINE_CURVE(5,(#17255,#17256,#17257,#17258,#17259,#17260,#17261,#17262,
#17263,#17264,#17265,#17266,#17267,#17268,#17269,#17270,#17271,#17272,#17273,
#17274,#17275,#17276,#17277,#17278,#17279,#17280,#17281,#17282,#17283,#17284,
#17285,#17286,#17287,#17288,#17289),.UNSPECIFIED.,.F.,.F.)
B_SPLINE_CURVE_WITH_KNOTS((6,1,1,1,1,1,1,1,1,1,1,1,1,1,1,1,1,1,1,1,1,1,
1,1,1,1,1,1,1,1,6),(0.,0.0333333333333333,0.0666666666666667,0.1,0.133333333333333,
0.166666666666667,0.2,0.233333333333333,0.266666666666667,0.3,0.333333333333333,
0.366666666666667,0.4,0.433333333333333,0.466666666666667,0.5,0.533333333333333,
0.566666666666667,0.6,0.633333333333333,0.666666666666667,0.7,0.733333333333333,
0.766666666666667,0.8,0.833333333333333,0.866666666666667,0.9,0.933333333333333,
0.966666666666667,1.),.UNSPECIFIED.)
CURVE()
GEOMETRIC_REPRESENTATION_ITEM()
RATIONAL_B_SPLINE_CURVE((1.,1.,1.,1.,1.,1.,1.,1.,1.,1.,1.,1.,1.,1.,1.,1.,
1.,1.,1.,1.,1.,1.,1.,1.,1.,1.,1.,1.,1.,1.,1.,1.,1.,1.,1.))
REPRESENTATION_ITEM('')
);
#289=(
BOUNDED_CURVE()
B_SPLINE_CURVE(5,(#17293,#17294,#17295,#17296,#17297,#17298,#17299,#17300,
#17301,#17302,#17303,#17304,#17305,#17306,#17307,#17308,#17309,#17310,#17311,
#17312,#17313,#17314,#17315,#17316,#17317,#17318,#17319,#17320,#17321,#17322,
#17323,#17324,#17325,#17326,#17327),.UNSPECIFIED.,.F.,.F.)
B_SPLINE_CURVE_WITH_KNOTS((6,1,1,1,1,1,1,1,1,1,1,1,1,1,1,1,1,1,1,1,1,1,
1,1,1,1,1,1,1,1,6),(0.,0.0333333333333333,0.0666666666666667,0.1,0.133333333333333,
0.166666666666667,0.2,0.233333333333333,0.266666666666667,0.3,0.333333333333333,
0.366666666666667,0.4,0.433333333333333,0.466666666666667,0.5,0.533333333333333,
0.566666666666667,0.6,0.633333333333333,0.666666666666667,0.7,0.733333333333333,
0.766666666666667,0.8,0.833333333333333,0.866666666666667,0.9,0.933333333333333,
0.966666666666667,1.),.UNSPECIFIED.)
CURVE()
GEOMETRIC_REPRESENTATION_ITEM()
RATIONAL_B_SPLINE_CURVE((1.,1.,1.,1.,1.,1.,1.,1.,1.,1.,1.,1.,1.,1.,1.,1.,
1.,1.,1.,1.,1.,1.,1.,1.,1.,1.,1.,1.,1.,1.,1.,1.,1.,1.,1.))
REPRESENTATION_ITEM('')
);
#290=(
BOUNDED_CURVE()
B_SPLINE_CURVE(5,(#17329,#17330,#17331,#17332,#17333,#17334,#17335,#17336,
#17337,#17338,#17339,#17340,#17341,#17342,#17343,#17344,#17345,#17346,#17347,
#17348,#17349,#17350,#17351,#17352,#17353,#17354,#17355,#17356,#17357,#17358,
#17359,#17360,#17361,#17362,#17363),.UNSPECIFIED.,.F.,.F.)
B_SPLINE_CURVE_WITH_KNOTS((6,1,1,1,1,1,1,1,1,1,1,1,1,1,1,1,1,1,1,1,1,1,
1,1,1,1,1,1,1,1,6),(0.,0.0333333333333333,0.0666666666666667,0.1,0.133333333333333,
0.166666666666667,0.2,0.233333333333333,0.266666666666667,0.3,0.333333333333333,
0.366666666666667,0.4,0.433333333333333,0.466666666666667,0.5,0.533333333333333,
0.566666666666667,0.6,0.633333333333333,0.666666666666667,0.7,0.733333333333333,
0.766666666666667,0.8,0.833333333333333,0.866666666666667,0.9,0.933333333333333,
0.966666666666667,1.),.UNSPECIFIED.)
CURVE()
GEOMETRIC_REPRESENTATION_ITEM()
RATIONAL_B_SPLINE_CURVE((1.,1.,1.,1.,1.,1.,1.,1.,1.,1.,1.,1.,1.,1.,1.,1.,
1.,1.,1.,1.,1.,1.,1.,1.,1.,1.,1.,1.,1.,1.,1.,1.,1.,1.,1.))
REPRESENTATION_ITEM('')
);
#291=(
BOUNDED_CURVE()
B_SPLINE_CURVE(5,(#17367,#17368,#17369,#17370,#17371,#17372,#17373,#17374,
#17375,#17376,#17377,#17378,#17379,#17380,#17381,#17382,#17383,#17384,#17385,
#17386,#17387,#17388,#17389,#17390,#17391,#17392,#17393,#17394,#17395,#17396,
#17397,#17398,#17399,#17400,#17401),.UNSPECIFIED.,.F.,.F.)
B_SPLINE_CURVE_WITH_KNOTS((6,1,1,1,1,1,1,1,1,1,1,1,1,1,1,1,1,1,1,1,1,1,
1,1,1,1,1,1,1,1,6),(0.,0.0333333333333333,0.0666666666666667,0.1,0.133333333333333,
0.166666666666667,0.2,0.233333333333333,0.266666666666667,0.3,0.333333333333333,
0.366666666666667,0.4,0.433333333333333,0.466666666666667,0.5,0.533333333333333,
0.566666666666667,0.6,0.633333333333333,0.666666666666667,0.7,0.733333333333333,
0.766666666666667,0.8,0.833333333333333,0.866666666666667,0.9,0.933333333333333,
0.966666666666667,1.),.UNSPECIFIED.)
CURVE()
GEOMETRIC_REPRESENTATION_ITEM()
RATIONAL_B_SPLINE_CURVE((1.,1.,1.,1.,1.,1.,1.,1.,1.,1.,1.,1.,1.,1.,1.,1.,
1.,1.,1.,1.,1.,1.,1.,1.,1.,1.,1.,1.,1.,1.,1.,1.,1.,1.,1.))
REPRESENTATION_ITEM('')
);
#292=(
BOUNDED_CURVE()
B_SPLINE_CURVE(5,(#17403,#17404,#17405,#17406,#17407,#17408,#17409,#17410,
#17411,#17412,#17413,#17414,#17415,#17416,#17417,#17418,#17419,#17420,#17421,
#17422,#17423,#17424,#17425,#17426,#17427,#17428,#17429,#17430,#17431,#17432,
#17433,#17434,#17435,#17436,#17437),.UNSPECIFIED.,.F.,.F.)
B_SPLINE_CURVE_WITH_KNOTS((6,1,1,1,1,1,1,1,1,1,1,1,1,1,1,1,1,1,1,1,1,1,
1,1,1,1,1,1,1,1,6),(0.,0.0333333333333333,0.0666666666666667,0.1,0.133333333333333,
0.166666666666667,0.2,0.233333333333333,0.266666666666667,0.3,0.333333333333333,
0.366666666666667,0.4,0.433333333333333,0.466666666666667,0.5,0.533333333333333,
0.566666666666667,0.6,0.633333333333333,0.666666666666667,0.7,0.733333333333333,
0.766666666666667,0.8,0.833333333333333,0.866666666666667,0.9,0.933333333333333,
0.966666666666667,1.),.UNSPECIFIED.)
CURVE()
GEOMETRIC_REPRESENTATION_ITEM()
RATIONAL_B_SPLINE_CURVE((1.,1.,1.,1.,1.,1.,1.,1.,1.,1.,1.,1.,1.,1.,1.,1.,
1.,1.,1.,1.,1.,1.,1.,1.,1.,1.,1.,1.,1.,1.,1.,1.,1.,1.,1.))
REPRESENTATION_ITEM('')
);
#293=(
BOUNDED_CURVE()
B_SPLINE_CURVE(5,(#17441,#17442,#17443,#17444,#17445,#17446,#17447,#17448,
#17449,#17450,#17451,#17452,#17453,#17454,#17455,#17456,#17457,#17458,#17459,
#17460,#17461,#17462,#17463,#17464,#17465,#17466,#17467,#17468,#17469,#17470,
#17471,#17472,#17473,#17474,#17475),.UNSPECIFIED.,.F.,.F.)
B_SPLINE_CURVE_WITH_KNOTS((6,1,1,1,1,1,1,1,1,1,1,1,1,1,1,1,1,1,1,1,1,1,
1,1,1,1,1,1,1,1,6),(0.,0.0333333333333333,0.0666666666666667,0.1,0.133333333333333,
0.166666666666667,0.2,0.233333333333333,0.266666666666667,0.3,0.333333333333333,
0.366666666666667,0.4,0.433333333333333,0.466666666666667,0.5,0.533333333333333,
0.566666666666667,0.6,0.633333333333333,0.666666666666667,0.7,0.733333333333333,
0.766666666666667,0.8,0.833333333333333,0.866666666666667,0.9,0.933333333333333,
0.966666666666667,1.),.UNSPECIFIED.)
CURVE()
GEOMETRIC_REPRESENTATION_ITEM()
RATIONAL_B_SPLINE_CURVE((1.,1.,1.,1.,1.,1.,1.,1.,1.,1.,1.,1.,1.,1.,1.,1.,
1.,1.,1.,1.,1.,1.,1.,1.,1.,1.,1.,1.,1.,1.,1.,1.,1.,1.,1.))
REPRESENTATION_ITEM('')
);
#294=(
BOUNDED_CURVE()
B_SPLINE_CURVE(5,(#17476,#17477,#17478,#17479,#17480,#17481,#17482,#17483,
#17484,#17485,#17486,#17487,#17488,#17489,#17490,#17491,#17492,#17493,#17494,
#17495,#17496,#17497,#17498,#17499,#17500,#17501,#17502,#17503,#17504,#17505,
#17506,#17507,#17508,#17509,#17510),.UNSPECIFIED.,.F.,.F.)
B_SPLINE_CURVE_WITH_KNOTS((6,1,1,1,1,1,1,1,1,1,1,1,1,1,1,1,1,1,1,1,1,1,
1,1,1,1,1,1,1,1,6),(0.,0.0333333333333333,0.0666666666666667,0.1,0.133333333333333,
0.166666666666667,0.2,0.233333333333333,0.266666666666667,0.3,0.333333333333333,
0.366666666666667,0.4,0.433333333333333,0.466666666666667,0.5,0.533333333333333,
0.566666666666667,0.6,0.633333333333333,0.666666666666667,0.7,0.733333333333333,
0.766666666666667,0.8,0.833333333333333,0.866666666666667,0.9,0.933333333333333,
0.966666666666667,1.),.UNSPECIFIED.)
CURVE()
GEOMETRIC_REPRESENTATION_ITEM()
RATIONAL_B_SPLINE_CURVE((1.,1.,1.,1.,1.,1.,1.,1.,1.,1.,1.,1.,1.,1.,1.,1.,
1.,1.,1.,1.,1.,1.,1.,1.,1.,1.,1.,1.,1.,1.,1.,1.,1.,1.,1.))
REPRESENTATION_ITEM('')
);
#295=(
BOUNDED_CURVE()
B_SPLINE_CURVE(5,(#18173,#18174,#18175,#18176,#18177,#18178),
 .UNSPECIFIED.,.F.,.F.)
B_SPLINE_CURVE_WITH_KNOTS((6,6),(0.,0.0167044419729414),.UNSPECIFIED.)
CURVE()
GEOMETRIC_REPRESENTATION_ITEM()
RATIONAL_B_SPLINE_CURVE((1.,1.,1.,1.,1.,1.))
REPRESENTATION_ITEM('')
);
#296=(
BOUNDED_CURVE()
B_SPLINE_CURVE(5,(#18233,#18234,#18235,#18236,#18237,#18238),
 .UNSPECIFIED.,.F.,.F.)
B_SPLINE_CURVE_WITH_KNOTS((6,6),(0.,0.0167044419729412),.UNSPECIFIED.)
CURVE()
GEOMETRIC_REPRESENTATION_ITEM()
RATIONAL_B_SPLINE_CURVE((1.,1.,1.,1.,1.,1.))
REPRESENTATION_ITEM('')
);
#297=(
BOUNDED_CURVE()
B_SPLINE_CURVE(5,(#18293,#18294,#18295,#18296,#18297,#18298),
 .UNSPECIFIED.,.F.,.F.)
B_SPLINE_CURVE_WITH_KNOTS((6,6),(0.,0.016704441972942),.UNSPECIFIED.)
CURVE()
GEOMETRIC_REPRESENTATION_ITEM()
RATIONAL_B_SPLINE_CURVE((1.,1.,1.,1.,1.,1.))
REPRESENTATION_ITEM('')
);
#298=(
BOUNDED_CURVE()
B_SPLINE_CURVE(5,(#18353,#18354,#18355,#18356,#18357,#18358),
 .UNSPECIFIED.,.F.,.F.)
B_SPLINE_CURVE_WITH_KNOTS((6,6),(0.,0.0167044419729414),.UNSPECIFIED.)
CURVE()
GEOMETRIC_REPRESENTATION_ITEM()
RATIONAL_B_SPLINE_CURVE((1.,1.,1.,1.,1.,1.))
REPRESENTATION_ITEM('')
);
#299=(
BOUNDED_CURVE()
B_SPLINE_CURVE(5,(#18413,#18414,#18415,#18416,#18417,#18418),
 .UNSPECIFIED.,.F.,.F.)
B_SPLINE_CURVE_WITH_KNOTS((6,6),(0.,0.0167044419729419),.UNSPECIFIED.)
CURVE()
GEOMETRIC_REPRESENTATION_ITEM()
RATIONAL_B_SPLINE_CURVE((1.,1.,1.,1.,1.,1.))
REPRESENTATION_ITEM('')
);
#300=(
BOUNDED_CURVE()
B_SPLINE_CURVE(5,(#18473,#18474,#18475,#18476,#18477,#18478),
 .UNSPECIFIED.,.F.,.F.)
B_SPLINE_CURVE_WITH_KNOTS((6,6),(0.,0.0167044419729413),.UNSPECIFIED.)
CURVE()
GEOMETRIC_REPRESENTATION_ITEM()
RATIONAL_B_SPLINE_CURVE((1.,1.,1.,1.,1.,1.))
REPRESENTATION_ITEM('')
);
#301=(
BOUNDED_CURVE()
B_SPLINE_CURVE(5,(#18533,#18534,#18535,#18536,#18537,#18538),
 .UNSPECIFIED.,.F.,.F.)
B_SPLINE_CURVE_WITH_KNOTS((6,6),(0.,0.016704441972941),.UNSPECIFIED.)
CURVE()
GEOMETRIC_REPRESENTATION_ITEM()
RATIONAL_B_SPLINE_CURVE((1.,1.,1.,1.,1.,1.))
REPRESENTATION_ITEM('')
);
#302=(
BOUNDED_CURVE()
B_SPLINE_CURVE(5,(#18593,#18594,#18595,#18596,#18597,#18598),
 .UNSPECIFIED.,.F.,.F.)
B_SPLINE_CURVE_WITH_KNOTS((6,6),(0.,0.0167044419729416),.UNSPECIFIED.)
CURVE()
GEOMETRIC_REPRESENTATION_ITEM()
RATIONAL_B_SPLINE_CURVE((1.,1.,1.,1.,1.,1.))
REPRESENTATION_ITEM('')
);
#303=(
BOUNDED_CURVE()
B_SPLINE_CURVE(5,(#18653,#18654,#18655,#18656,#18657,#18658),
 .UNSPECIFIED.,.F.,.F.)
B_SPLINE_CURVE_WITH_KNOTS((6,6),(0.,0.0167044419729408),.UNSPECIFIED.)
CURVE()
GEOMETRIC_REPRESENTATION_ITEM()
RATIONAL_B_SPLINE_CURVE((1.,1.,1.,1.,1.,1.))
REPRESENTATION_ITEM('')
);
#304=(
BOUNDED_CURVE()
B_SPLINE_CURVE(5,(#18713,#18714,#18715,#18716,#18717,#18718),
 .UNSPECIFIED.,.F.,.F.)
B_SPLINE_CURVE_WITH_KNOTS((6,6),(0.,0.0167044419729419),.UNSPECIFIED.)
CURVE()
GEOMETRIC_REPRESENTATION_ITEM()
RATIONAL_B_SPLINE_CURVE((1.,1.,1.,1.,1.,1.))
REPRESENTATION_ITEM('')
);
#305=(
BOUNDED_CURVE()
B_SPLINE_CURVE(5,(#18773,#18774,#18775,#18776,#18777,#18778),
 .UNSPECIFIED.,.F.,.F.)
B_SPLINE_CURVE_WITH_KNOTS((6,6),(0.,0.016704441972942),.UNSPECIFIED.)
CURVE()
GEOMETRIC_REPRESENTATION_ITEM()
RATIONAL_B_SPLINE_CURVE((1.,1.,1.,1.,1.,1.))
REPRESENTATION_ITEM('')
);
#306=(
BOUNDED_CURVE()
B_SPLINE_CURVE(5,(#18833,#18834,#18835,#18836,#18837,#18838),
 .UNSPECIFIED.,.F.,.F.)
B_SPLINE_CURVE_WITH_KNOTS((6,6),(0.,0.016704441972941),.UNSPECIFIED.)
CURVE()
GEOMETRIC_REPRESENTATION_ITEM()
RATIONAL_B_SPLINE_CURVE((1.,1.,1.,1.,1.,1.))
REPRESENTATION_ITEM('')
);
#307=(
BOUNDED_CURVE()
B_SPLINE_CURVE(5,(#18893,#18894,#18895,#18896,#18897,#18898),
 .UNSPECIFIED.,.F.,.F.)
B_SPLINE_CURVE_WITH_KNOTS((6,6),(0.,0.0167044419729416),.UNSPECIFIED.)
CURVE()
GEOMETRIC_REPRESENTATION_ITEM()
RATIONAL_B_SPLINE_CURVE((1.,1.,1.,1.,1.,1.))
REPRESENTATION_ITEM('')
);
#308=(
BOUNDED_CURVE()
B_SPLINE_CURVE(5,(#18953,#18954,#18955,#18956,#18957,#18958),
 .UNSPECIFIED.,.F.,.F.)
B_SPLINE_CURVE_WITH_KNOTS((6,6),(0.,0.0167044419729408),.UNSPECIFIED.)
CURVE()
GEOMETRIC_REPRESENTATION_ITEM()
RATIONAL_B_SPLINE_CURVE((1.,1.,1.,1.,1.,1.))
REPRESENTATION_ITEM('')
);
#309=(
BOUNDED_CURVE()
B_SPLINE_CURVE(5,(#19013,#19014,#19015,#19016,#19017,#19018),
 .UNSPECIFIED.,.F.,.F.)
B_SPLINE_CURVE_WITH_KNOTS((6,6),(0.,0.0167044419729419),.UNSPECIFIED.)
CURVE()
GEOMETRIC_REPRESENTATION_ITEM()
RATIONAL_B_SPLINE_CURVE((1.,1.,1.,1.,1.,1.))
REPRESENTATION_ITEM('')
);
#310=(
BOUNDED_CURVE()
B_SPLINE_CURVE(5,(#19073,#19074,#19075,#19076,#19077,#19078),
 .UNSPECIFIED.,.F.,.F.)
B_SPLINE_CURVE_WITH_KNOTS((6,6),(0.,0.0167044419729415),.UNSPECIFIED.)
CURVE()
GEOMETRIC_REPRESENTATION_ITEM()
RATIONAL_B_SPLINE_CURVE((1.,1.,1.,1.,1.,1.))
REPRESENTATION_ITEM('')
);
#311=(
BOUNDED_CURVE()
B_SPLINE_CURVE(5,(#19133,#19134,#19135,#19136,#19137,#19138),
 .UNSPECIFIED.,.F.,.F.)
B_SPLINE_CURVE_WITH_KNOTS((6,6),(0.,0.0167044419729417),.UNSPECIFIED.)
CURVE()
GEOMETRIC_REPRESENTATION_ITEM()
RATIONAL_B_SPLINE_CURVE((1.,1.,1.,1.,1.,1.))
REPRESENTATION_ITEM('')
);
#312=(
BOUNDED_CURVE()
B_SPLINE_CURVE(5,(#19193,#19194,#19195,#19196,#19197,#19198),
 .UNSPECIFIED.,.F.,.F.)
B_SPLINE_CURVE_WITH_KNOTS((6,6),(0.,0.0167044419729418),.UNSPECIFIED.)
CURVE()
GEOMETRIC_REPRESENTATION_ITEM()
RATIONAL_B_SPLINE_CURVE((1.,1.,1.,1.,1.,1.))
REPRESENTATION_ITEM('')
);
#313=(
BOUNDED_CURVE()
B_SPLINE_CURVE(5,(#19253,#19254,#19255,#19256,#19257,#19258),
 .UNSPECIFIED.,.F.,.F.)
B_SPLINE_CURVE_WITH_KNOTS((6,6),(0.,0.0167044419729408),.UNSPECIFIED.)
CURVE()
GEOMETRIC_REPRESENTATION_ITEM()
RATIONAL_B_SPLINE_CURVE((1.,1.,1.,1.,1.,1.))
REPRESENTATION_ITEM('')
);
#314=(
BOUNDED_CURVE()
B_SPLINE_CURVE(5,(#19313,#19314,#19315,#19316,#19317,#19318),
 .UNSPECIFIED.,.F.,.F.)
B_SPLINE_CURVE_WITH_KNOTS((6,6),(0.,0.0167044419729419),.UNSPECIFIED.)
CURVE()
GEOMETRIC_REPRESENTATION_ITEM()
RATIONAL_B_SPLINE_CURVE((1.,1.,1.,1.,1.,1.))
REPRESENTATION_ITEM('')
);
#315=(
BOUNDED_CURVE()
B_SPLINE_CURVE(5,(#19364,#19365,#19366,#19367,#19368,#19369),
 .UNSPECIFIED.,.F.,.F.)
B_SPLINE_CURVE_WITH_KNOTS((6,6),(0.984324037881896,1.),.UNSPECIFIED.)
CURVE()
GEOMETRIC_REPRESENTATION_ITEM()
RATIONAL_B_SPLINE_CURVE((1.,1.,1.,1.,1.,1.))
REPRESENTATION_ITEM('')
);
#316=(
BOUNDED_CURVE()
B_SPLINE_CURVE(5,(#20018,#20019,#20020,#20021,#20022,#20023),
 .UNSPECIFIED.,.F.,.F.)
B_SPLINE_CURVE_WITH_KNOTS((6,6),(0.984324037881896,1.),.UNSPECIFIED.)
CURVE()
GEOMETRIC_REPRESENTATION_ITEM()
RATIONAL_B_SPLINE_CURVE((1.,1.,1.,1.,1.,1.))
REPRESENTATION_ITEM('')
);
#317=(
BOUNDED_CURVE()
B_SPLINE_CURVE(5,(#20073,#20074,#20075,#20076,#20077,#20078),
 .UNSPECIFIED.,.F.,.F.)
B_SPLINE_CURVE_WITH_KNOTS((6,6),(0.984324037881895,1.),.UNSPECIFIED.)
CURVE()
GEOMETRIC_REPRESENTATION_ITEM()
RATIONAL_B_SPLINE_CURVE((1.,1.,1.,1.,1.,1.))
REPRESENTATION_ITEM('')
);
#318=(
BOUNDED_CURVE()
B_SPLINE_CURVE(5,(#20128,#20129,#20130,#20131,#20132,#20133),
 .UNSPECIFIED.,.F.,.F.)
B_SPLINE_CURVE_WITH_KNOTS((6,6),(0.984324037881896,1.),.UNSPECIFIED.)
CURVE()
GEOMETRIC_REPRESENTATION_ITEM()
RATIONAL_B_SPLINE_CURVE((1.,1.,1.,1.,1.,1.))
REPRESENTATION_ITEM('')
);
#319=(
BOUNDED_CURVE()
B_SPLINE_CURVE(5,(#20179,#20180,#20181,#20182,#20183,#20184),
 .UNSPECIFIED.,.F.,.F.)
B_SPLINE_CURVE_WITH_KNOTS((6,6),(0.984324037881896,1.),.UNSPECIFIED.)
CURVE()
GEOMETRIC_REPRESENTATION_ITEM()
RATIONAL_B_SPLINE_CURVE((1.,1.,1.,1.,1.,1.))
REPRESENTATION_ITEM('')
);
#320=(
BOUNDED_CURVE()
B_SPLINE_CURVE(5,(#20230,#20231,#20232,#20233,#20234,#20235),
 .UNSPECIFIED.,.F.,.F.)
B_SPLINE_CURVE_WITH_KNOTS((6,6),(0.984324037881896,1.),.UNSPECIFIED.)
CURVE()
GEOMETRIC_REPRESENTATION_ITEM()
RATIONAL_B_SPLINE_CURVE((1.,1.,1.,1.,1.,1.))
REPRESENTATION_ITEM('')
);
#321=(
BOUNDED_CURVE()
B_SPLINE_CURVE(5,(#20281,#20282,#20283,#20284,#20285,#20286),
 .UNSPECIFIED.,.F.,.F.)
B_SPLINE_CURVE_WITH_KNOTS((6,6),(0.984324037881896,1.),.UNSPECIFIED.)
CURVE()
GEOMETRIC_REPRESENTATION_ITEM()
RATIONAL_B_SPLINE_CURVE((1.,1.,1.,1.,1.,1.))
REPRESENTATION_ITEM('')
);
#322=(
BOUNDED_CURVE()
B_SPLINE_CURVE(5,(#20336,#20337,#20338,#20339,#20340,#20341),
 .UNSPECIFIED.,.F.,.F.)
B_SPLINE_CURVE_WITH_KNOTS((6,6),(0.984324037881896,1.),.UNSPECIFIED.)
CURVE()
GEOMETRIC_REPRESENTATION_ITEM()
RATIONAL_B_SPLINE_CURVE((1.,1.,1.,1.,1.,1.))
REPRESENTATION_ITEM('')
);
#323=(
BOUNDED_CURVE()
B_SPLINE_CURVE(5,(#20391,#20392,#20393,#20394,#20395,#20396),
 .UNSPECIFIED.,.F.,.F.)
B_SPLINE_CURVE_WITH_KNOTS((6,6),(0.984324037881896,1.),.UNSPECIFIED.)
CURVE()
GEOMETRIC_REPRESENTATION_ITEM()
RATIONAL_B_SPLINE_CURVE((1.,1.,1.,1.,1.,1.))
REPRESENTATION_ITEM('')
);
#324=(
BOUNDED_CURVE()
B_SPLINE_CURVE(5,(#20442,#20443,#20444,#20445,#20446,#20447),
 .UNSPECIFIED.,.F.,.F.)
B_SPLINE_CURVE_WITH_KNOTS((6,6),(0.984324037881896,1.),.UNSPECIFIED.)
CURVE()
GEOMETRIC_REPRESENTATION_ITEM()
RATIONAL_B_SPLINE_CURVE((1.,1.,1.,1.,1.,1.))
REPRESENTATION_ITEM('')
);
#325=(
BOUNDED_CURVE()
B_SPLINE_CURVE(5,(#20493,#20494,#20495,#20496,#20497,#20498),
 .UNSPECIFIED.,.F.,.F.)
B_SPLINE_CURVE_WITH_KNOTS((6,6),(0.984324037881895,1.),.UNSPECIFIED.)
CURVE()
GEOMETRIC_REPRESENTATION_ITEM()
RATIONAL_B_SPLINE_CURVE((1.,1.,1.,1.,1.,1.))
REPRESENTATION_ITEM('')
);
#326=(
BOUNDED_CURVE()
B_SPLINE_CURVE(5,(#20544,#20545,#20546,#20547,#20548,#20549),
 .UNSPECIFIED.,.F.,.F.)
B_SPLINE_CURVE_WITH_KNOTS((6,6),(0.984324037881896,1.),.UNSPECIFIED.)
CURVE()
GEOMETRIC_REPRESENTATION_ITEM()
RATIONAL_B_SPLINE_CURVE((1.,1.,1.,1.,1.,1.))
REPRESENTATION_ITEM('')
);
#327=(
BOUNDED_CURVE()
B_SPLINE_CURVE(5,(#20599,#20600,#20601,#20602,#20603,#20604),
 .UNSPECIFIED.,.F.,.F.)
B_SPLINE_CURVE_WITH_KNOTS((6,6),(0.984324037881896,1.),.UNSPECIFIED.)
CURVE()
GEOMETRIC_REPRESENTATION_ITEM()
RATIONAL_B_SPLINE_CURVE((1.,1.,1.,1.,1.,1.))
REPRESENTATION_ITEM('')
);
#328=(
BOUNDED_CURVE()
B_SPLINE_CURVE(5,(#20654,#20655,#20656,#20657,#20658,#20659),
 .UNSPECIFIED.,.F.,.F.)
B_SPLINE_CURVE_WITH_KNOTS((6,6),(0.984324037881896,1.),.UNSPECIFIED.)
CURVE()
GEOMETRIC_REPRESENTATION_ITEM()
RATIONAL_B_SPLINE_CURVE((1.,1.,1.,1.,1.,1.))
REPRESENTATION_ITEM('')
);
#329=(
BOUNDED_CURVE()
B_SPLINE_CURVE(5,(#20705,#20706,#20707,#20708,#20709,#20710),
 .UNSPECIFIED.,.F.,.F.)
B_SPLINE_CURVE_WITH_KNOTS((6,6),(0.984324037881896,1.),.UNSPECIFIED.)
CURVE()
GEOMETRIC_REPRESENTATION_ITEM()
RATIONAL_B_SPLINE_CURVE((1.,1.,1.,1.,1.,1.))
REPRESENTATION_ITEM('')
);
#330=(
BOUNDED_CURVE()
B_SPLINE_CURVE(5,(#20756,#20757,#20758,#20759,#20760,#20761),
 .UNSPECIFIED.,.F.,.F.)
B_SPLINE_CURVE_WITH_KNOTS((6,6),(0.984324037881896,1.),.UNSPECIFIED.)
CURVE()
GEOMETRIC_REPRESENTATION_ITEM()
RATIONAL_B_SPLINE_CURVE((1.,1.,1.,1.,1.,1.))
REPRESENTATION_ITEM('')
);
#331=(
BOUNDED_CURVE()
B_SPLINE_CURVE(5,(#20807,#20808,#20809,#20810,#20811,#20812),
 .UNSPECIFIED.,.F.,.F.)
B_SPLINE_CURVE_WITH_KNOTS((6,6),(0.984324037881896,1.),.UNSPECIFIED.)
CURVE()
GEOMETRIC_REPRESENTATION_ITEM()
RATIONAL_B_SPLINE_CURVE((1.,1.,1.,1.,1.,1.))
REPRESENTATION_ITEM('')
);
#332=(
BOUNDED_CURVE()
B_SPLINE_CURVE(5,(#20862,#20863,#20864,#20865,#20866,#20867),
 .UNSPECIFIED.,.F.,.F.)
B_SPLINE_CURVE_WITH_KNOTS((6,6),(0.984324037881896,1.),.UNSPECIFIED.)
CURVE()
GEOMETRIC_REPRESENTATION_ITEM()
RATIONAL_B_SPLINE_CURVE((1.,1.,1.,1.,1.,1.))
REPRESENTATION_ITEM('')
);
#333=(
BOUNDED_CURVE()
B_SPLINE_CURVE(5,(#20917,#20918,#20919,#20920,#20921,#20922),
 .UNSPECIFIED.,.F.,.F.)
B_SPLINE_CURVE_WITH_KNOTS((6,6),(0.984324037881896,1.),.UNSPECIFIED.)
CURVE()
GEOMETRIC_REPRESENTATION_ITEM()
RATIONAL_B_SPLINE_CURVE((1.,1.,1.,1.,1.,1.))
REPRESENTATION_ITEM('')
);
#334=(
BOUNDED_CURVE()
B_SPLINE_CURVE(5,(#20968,#20969,#20970,#20971,#20972,#20973),
 .UNSPECIFIED.,.F.,.F.)
B_SPLINE_CURVE_WITH_KNOTS((6,6),(0.984324037881896,1.),.UNSPECIFIED.)
CURVE()
GEOMETRIC_REPRESENTATION_ITEM()
RATIONAL_B_SPLINE_CURVE((1.,1.,1.,1.,1.,1.))
REPRESENTATION_ITEM('')
);
#335=B_SPLINE_CURVE_WITH_KNOTS('',3,(#9770,#9771,#9772,#9773,#9774,#9775),
 .UNSPECIFIED.,.F.,.F.,(4,2,4),(0.150716059332096,0.396655662727104,0.79918856408106),
 .UNSPECIFIED.);
#336=B_SPLINE_CURVE_WITH_KNOTS('',3,(#9778,#9779,#9780,#9781),
 .UNSPECIFIED.,.F.,.F.,(4,4),(0.,0.07026331290575),.UNSPECIFIED.);
#337=B_SPLINE_CURVE_WITH_KNOTS('',3,(#9785,#9786,#9787,#9788,#9789,#9790,
#9791,#9792,#9793,#9794),.UNSPECIFIED.,.F.,.F.,(4,2,2,2,4),(0.331186461688063,
0.41497096063171,0.498755459575358,0.580564191475742,0.662372923376126),
 .UNSPECIFIED.);
#338=B_SPLINE_CURVE_WITH_KNOTS('',3,(#9796,#9797,#9798,#9799,#9800,#9801,
#9802,#9803,#9804,#9805,#9806,#9807,#9808,#9809,#9810,#9811,#9812,#9813,
#9814),.UNSPECIFIED.,.F.,.F.,(4,2,2,2,3,2,2,2,4),(0.993559385064188,1.07734388400784,
1.16112838295148,1.24293711485187,1.32474584675225,1.40655457865263,1.48836331055302,
1.57214780949667,1.65593230844031),.UNSPECIFIED.);
#339=B_SPLINE_CURVE_WITH_KNOTS('',3,(#9815,#9816,#9817,#9818,#9819,#9820,
#9821,#9822,#9823,#9824),.UNSPECIFIED.,.F.,.F.,(4,2,2,2,4),(0.662372923376126,
0.744181655276509,0.825990387176893,0.909774886120541,0.993559385064188),
 .UNSPECIFIED.);
#340=B_SPLINE_CURVE_WITH_KNOTS('',3,(#9832,#9833,#9834,#9835,#9836,#9837,
#9838,#9839,#9840,#9841),.UNSPECIFIED.,.F.,.F.,(4,2,2,2,4),(0.934777550778115,
1.01265597092338,1.09053439106865,1.1684522293864,1.24637006770415),
 .UNSPECIFIED.);
#341=B_SPLINE_CURVE_WITH_KNOTS('',3,(#9843,#9844,#9845,#9846,#9847,#9848,
#9849,#9850,#9851,#9852,#9853,#9854,#9855,#9856,#9857,#9858,#9859,#9860),
 .UNSPECIFIED.,.F.,.F.,(4,2,2,2,2,2,2,2,4),(0.311592516926038,0.389470937071308,
0.467349357216578,0.545267195534327,0.623185033852077,0.701102872169826,
0.779020710487576,0.856899130632846,0.934777550778115),.UNSPECIFIED.);
#342=B_SPLINE_CURVE_WITH_KNOTS('',3,(#9861,#9862,#9863,#9864,#9865,#9866,
#9867,#9868,#9869,#9870),.UNSPECIFIED.,.F.,.F.,(4,2,2,2,4),(0.,0.0779178383177495,
0.155835676635499,0.233714096780769,0.311592516926038),.UNSPECIFIED.);
#343=B_SPLINE_CURVE_WITH_KNOTS('',3,(#9874,#9875,#9876,#9877,#9878,#9879,
#9880,#9881,#9882,#9883,#9884,#9885,#9886,#9887,#9888,#9889,#9890,#9891),
 .UNSPECIFIED.,.F.,.F.,(4,2,2,2,2,2,2,2,4),(0.331186461688063,0.41497096063171,
0.498755459575358,0.580564191475742,0.662372923376126,0.744181655276509,
0.825990387176893,0.909774886120541,0.993559385064188),.UNSPECIFIED.);
#344=B_SPLINE_CURVE_WITH_KNOTS('',3,(#9895,#9896,#9897,#9898,#9899,#9900,
#9901,#9902,#9903,#9904,#9905,#9906,#9907,#9908,#9909,#9910,#9911,#9912,
#9913),.UNSPECIFIED.,.F.,.F.,(4,2,2,2,3,2,2,2,4),(0.993559385064188,1.07734388400784,
1.16112838295148,1.24293711485187,1.32474584675225,1.40655457865263,1.48836331055302,
1.57214780949667,1.65593230844031),.UNSPECIFIED.);
#345=B_SPLINE_CURVE_WITH_KNOTS('',3,(#9918,#9919,#9920,#9921,#9922,#9923,
#9924,#9925,#9926,#9927),.UNSPECIFIED.,.F.,.F.,(4,2,2,2,4),(0.,0.0779178383177495,
0.155835676635499,0.233714096780769,0.311592516926038),.UNSPECIFIED.);
#346=B_SPLINE_CURVE_WITH_KNOTS('',3,(#9928,#9929,#9930,#9931,#9932,#9933,
#9934,#9935,#9936,#9937,#9938,#9939,#9940,#9941,#9942,#9943,#9944,#9945,
#9946,#9947,#9948,#9949,#9950,#9951,#9952,#9953),.UNSPECIFIED.,.F.,.F.,
(4,2,2,2,2,2,2,2,2,2,2,2,4),(0.311592516926038,0.389470937071308,0.467349357216578,
0.545267195534327,0.623185033852077,0.701102872169826,0.779020710487576,
0.856899130632846,0.934777550778115,1.01265597092338,1.09053439106865,1.1684522293864,
1.24637006770415),.UNSPECIFIED.);
#347=B_SPLINE_CURVE_WITH_KNOTS('',3,(#11468,#11469,#11470,#11471,#11472,
#11473,#11474,#11475,#11476,#11477,#11478,#11479,#11480,#11481,#11482,#11483),
 .UNSPECIFIED.,.F.,.F.,(4,2,2,2,2,2,2,4),(-0.530628370665211,-0.438179590528544,
-0.368258168563918,-0.304848975856517,-0.18363749529654,-0.110124331620288,
-0.0450078568694679,0.),.UNSPECIFIED.);
#348=B_SPLINE_CURVE_WITH_KNOTS('',3,(#11485,#11486,#11487,#11488,#11489,
#11490,#11491,#11492,#11493,#11494),.UNSPECIFIED.,.F.,.F.,(4,2,2,2,4),(-0.385870474914649,
-0.314059136023987,-0.239369291310806,-0.135126671385033,0.),
 .UNSPECIFIED.);
#349=B_SPLINE_CURVE_WITH_KNOTS('',3,(#11499,#11500,#11501,#11502,#11503,
#11504,#11505,#11506,#11507,#11508,#11509,#11510,#11511,#11512,#11513,#11514),
 .UNSPECIFIED.,.F.,.F.,(4,2,2,2,2,2,2,4),(-0.530628370644343,-0.438179590518134,
-0.368258168560348,-0.304848975855471,-0.183637495295765,-0.110124331619939,
-0.0450078568693863,0.),.UNSPECIFIED.);
#350=B_SPLINE_CURVE_WITH_KNOTS('',3,(#11516,#11517,#11518,#11519,#11520,
#11521,#11522,#11523,#11524,#11525),.UNSPECIFIED.,.F.,.F.,(4,2,2,2,4),(-0.385870474933965,
-0.314059136035213,-0.239369291313655,-0.135126671384286,0.),
 .UNSPECIFIED.);
#351=B_SPLINE_CURVE_WITH_KNOTS('',3,(#11530,#11531,#11532,#11533,#11534,
#11535,#11536,#11537,#11538,#11539,#11540,#11541,#11542,#11543,#11544,#11545),
 .UNSPECIFIED.,.F.,.F.,(4,2,2,2,2,2,2,4),(-0.530628370635536,-0.438179590504702,
-0.368258168546477,-0.304848975844171,-0.183637495294767,-0.110124331621409,
-0.0450078568700918,0.),.UNSPECIFIED.);
#352=B_SPLINE_CURVE_WITH_KNOTS('',3,(#11547,#11548,#11549,#11550,#11551,
#11552,#11553,#11554,#11555,#11556),.UNSPECIFIED.,.F.,.F.,(4,2,2,2,4),(-0.38587047497607,
-0.314059136063502,-0.239369291327215,-0.135126671388375,0.),
 .UNSPECIFIED.);
#353=B_SPLINE_CURVE_WITH_KNOTS('',3,(#11561,#11562,#11563,#11564,#11565,
#11566,#11567,#11568,#11569,#11570,#11571,#11572,#11573,#11574,#11575,#11576),
 .UNSPECIFIED.,.F.,.F.,(4,2,2,2,2,2,2,4),(-0.530628370675815,-0.438179590528513,
-0.368258168562559,-0.304848975858297,-0.18363749529809,-0.110124331620912,
-0.0450078568696886,0.),.UNSPECIFIED.);
#354=B_SPLINE_CURVE_WITH_KNOTS('',3,(#11578,#11579,#11580,#11581,#11582,
#11583,#11584,#11585,#11586,#11587),.UNSPECIFIED.,.F.,.F.,(4,2,2,2,4),(-0.38587047490018,
-0.31405913601548,-0.239369291308653,-0.135126671385624,0.),
 .UNSPECIFIED.);
#355=B_SPLINE_CURVE_WITH_KNOTS('',3,(#11592,#11593,#11594,#11595,#11596,
#11597,#11598,#11599,#11600,#11601,#11602,#11603,#11604,#11605,#11606,#11607),
 .UNSPECIFIED.,.F.,.F.,(4,2,2,2,2,2,2,4),(-0.530628370637572,-0.438179590515746,
-0.36825816856043,-0.304848975855941,-0.183637495296692,-0.11012433162041,
-0.0450078568695264,0.),.UNSPECIFIED.);
#356=B_SPLINE_CURVE_WITH_KNOTS('',3,(#11609,#11610,#11611,#11612,#11613,
#11614,#11615,#11616,#11617,#11618),.UNSPECIFIED.,.F.,.F.,(4,2,2,2,4),(-0.385870474947031,
-0.314059136043926,-0.239369291317936,-0.135126671385535,0.),
 .UNSPECIFIED.);
#357=B_SPLINE_CURVE_WITH_KNOTS('',3,(#11623,#11624,#11625,#11626,#11627,
#11628,#11629,#11630,#11631,#11632,#11633,#11634,#11635,#11636,#11637,#11638),
 .UNSPECIFIED.,.F.,.F.,(4,2,2,2,2,2,2,4),(-0.530628370654682,-0.438179590523996,
-0.368258168563118,-0.304848975857009,-0.18363749529649,-0.11012433162027,
-0.0450078568694597,0.),.UNSPECIFIED.);
#358=B_SPLINE_CURVE_WITH_KNOTS('',3,(#11640,#11641,#11642,#11643,#11644,
#11645,#11646,#11647,#11648,#11649),.UNSPECIFIED.,.F.,.F.,(4,2,2,2,4),(-0.385870474959562,
-0.314059136052487,-0.239369291321785,-0.135126671386547,0.),
 .UNSPECIFIED.);
#359=B_SPLINE_CURVE_WITH_KNOTS('',3,(#11654,#11655,#11656,#11657,#11658,
#11659,#11660,#11661,#11662,#11663,#11664,#11665,#11666,#11667,#11668,#11669),
 .UNSPECIFIED.,.F.,.F.,(4,2,2,2,2,2,2,4),(-0.530628370674281,-0.438179590531451,
-0.368258168567116,-0.304848975861869,-0.183637495299954,-0.110124331621691,
-0.0450078568699812,0.),.UNSPECIFIED.);
#360=B_SPLINE_CURVE_WITH_KNOTS('',3,(#11671,#11672,#11673,#11674,#11675,
#11676,#11677,#11678,#11679,#11680),.UNSPECIFIED.,.F.,.F.,(4,2,2,2,4),(-0.385870474910037,
-0.314059136021404,-0.239369291308962,-0.135126671384126,0.),
 .UNSPECIFIED.);
#361=B_SPLINE_CURVE_WITH_KNOTS('',3,(#11685,#11686,#11687,#11688,#11689,
#11690,#11691,#11692,#11693,#11694,#11695,#11696,#11697,#11698,#11699,#11700),
 .UNSPECIFIED.,.F.,.F.,(4,2,2,2,2,2,2,4),(-0.530628370695727,-0.438179590541344,
-0.368258168569252,-0.304848975860891,-0.183637495301317,-0.110124331622579,
-0.0450078568703517,0.),.UNSPECIFIED.);
#362=B_SPLINE_CURVE_WITH_KNOTS('',3,(#11702,#11703,#11704,#11705,#11706,
#11707,#11708,#11709,#11710,#11711),.UNSPECIFIED.,.F.,.F.,(4,2,2,2,4),(-0.385870474968525,
-0.314059136057782,-0.239369291326298,-0.135126671389261,0.),
 .UNSPECIFIED.);
#363=B_SPLINE_CURVE_WITH_KNOTS('',3,(#11716,#11717,#11718,#11719,#11720,
#11721,#11722,#11723,#11724,#11725,#11726,#11727,#11728,#11729,#11730,#11731),
 .UNSPECIFIED.,.F.,.F.,(4,2,2,2,2,2,2,4),(-0.530628370650825,-0.438179590522418,
-0.368258168560991,-0.304848975853564,-0.183637495295637,-0.110124331620217,
-0.0450078568694996,0.),.UNSPECIFIED.);
#364=B_SPLINE_CURVE_WITH_KNOTS('',3,(#11733,#11734,#11735,#11736,#11737,
#11738,#11739,#11740,#11741,#11742),.UNSPECIFIED.,.F.,.F.,(4,2,2,2,4),(-0.385870474779879,
-0.314059135940437,-0.239369291280562,-0.135126671382187,0.),
 .UNSPECIFIED.);
#365=B_SPLINE_CURVE_WITH_KNOTS('',3,(#11747,#11748,#11749,#11750,#11751,
#11752,#11753,#11754,#11755,#11756,#11757,#11758,#11759,#11760,#11761,#11762),
 .UNSPECIFIED.,.F.,.F.,(4,2,2,2,2,2,2,4),(-0.530628370676019,-0.438179590538652,
-0.36825816857226,-0.30484897586235,-0.1836374952988,-0.110124331620691,
-0.0450078568695567,0.),.UNSPECIFIED.);
#366=B_SPLINE_CURVE_WITH_KNOTS('',3,(#11764,#11765,#11766,#11767,#11768,
#11769,#11770,#11771,#11772,#11773),.UNSPECIFIED.,.F.,.F.,(4,2,2,2,4),(-0.385870474961872,
-0.314059136052803,-0.23936929132047,-0.135126671385201,0.),
 .UNSPECIFIED.);
#367=B_SPLINE_CURVE_WITH_KNOTS('',3,(#11778,#11779,#11780,#11781,#11782,
#11783,#11784,#11785,#11786,#11787,#11788,#11789,#11790,#11791,#11792,#11793),
 .UNSPECIFIED.,.F.,.F.,(4,2,2,2,2,2,2,4),(-0.530628370643928,-0.43817959051309,
-0.368258168552352,-0.30484897584762,-0.183637495292806,-0.110124331619433,
-0.0450078568692464,0.),.UNSPECIFIED.);
#368=B_SPLINE_CURVE_WITH_KNOTS('',3,(#11795,#11796,#11797,#11798,#11799,
#11800,#11801,#11802,#11803,#11804),.UNSPECIFIED.,.F.,.F.,(4,2,2,2,4),(-0.385870474963212,
-0.314059136054532,-0.239369291322363,-0.135126671386519,0.),
 .UNSPECIFIED.);
#369=B_SPLINE_CURVE_WITH_KNOTS('',3,(#11809,#11810,#11811,#11812,#11813,
#11814,#11815,#11816,#11817,#11818,#11819,#11820,#11821,#11822,#11823,#11824),
 .UNSPECIFIED.,.F.,.F.,(4,2,2,2,2,2,2,4),(-0.530628370650933,-0.438179590512731,
-0.368258168547674,-0.304848975842705,-0.18363749528933,-0.110124331617902,
-0.045007856868715,0.),.UNSPECIFIED.);
#370=B_SPLINE_CURVE_WITH_KNOTS('',3,(#11826,#11827,#11828,#11829,#11830,
#11831,#11832,#11833,#11834,#11835),.UNSPECIFIED.,.F.,.F.,(4,2,2,2,4),(-0.385870475012667,
-0.314059136085294,-0.239369291335385,-0.135126671389136,0.),
 .UNSPECIFIED.);
#371=B_SPLINE_CURVE_WITH_KNOTS('',3,(#11840,#11841,#11842,#11843,#11844,
#11845,#11846,#11847,#11848,#11849,#11850,#11851,#11852,#11853,#11854,#11855),
 .UNSPECIFIED.,.F.,.F.,(4,2,2,2,2,2,2,4),(-0.530628370751346,-0.438179590589213,
-0.368258168607749,-0.304848975890323,-0.183637495306509,-0.110124331620972,
-0.0450078568692966,0.),.UNSPECIFIED.);
#372=B_SPLINE_CURVE_WITH_KNOTS('',3,(#11857,#11858,#11859,#11860,#11861,
#11862,#11863,#11864,#11865,#11866),.UNSPECIFIED.,.F.,.F.,(4,2,2,2,4),(-0.38587047498259,
-0.314059136066901,-0.239369291329437,-0.135126671389429,0.),
 .UNSPECIFIED.);
#373=B_SPLINE_CURVE_WITH_KNOTS('',3,(#11871,#11872,#11873,#11874,#11875,
#11876,#11877,#11878,#11879,#11880,#11881,#11882,#11883,#11884,#11885,#11886),
 .UNSPECIFIED.,.F.,.F.,(4,2,2,2,2,2,2,4),(-0.5306283706486,-0.438179590513393,
-0.368258168552838,-0.304848975849369,-0.183637495296429,-0.110124331621205,
-0.0450078568699516,0.),.UNSPECIFIED.);
#374=B_SPLINE_CURVE_WITH_KNOTS('',3,(#11888,#11889,#11890,#11891,#11892,
#11893,#11894,#11895,#11896,#11897),.UNSPECIFIED.,.F.,.F.,(4,2,2,2,4),(-0.385870474786871,
-0.314059135944633,-0.23936929128179,-0.135126671382188,0.),
 .UNSPECIFIED.);
#375=B_SPLINE_CURVE_WITH_KNOTS('',3,(#11902,#11903,#11904,#11905,#11906,
#11907,#11908,#11909,#11910,#11911,#11912,#11913,#11914,#11915,#11916,#11917),
 .UNSPECIFIED.,.F.,.F.,(4,2,2,2,2,2,2,4),(-0.530628370663462,-0.438179590525026,
-0.368258168561372,-0.304848975855513,-0.183637495296643,-0.110124331620531,
-0.0450078568695819,0.),.UNSPECIFIED.);
#376=B_SPLINE_CURVE_WITH_KNOTS('',3,(#11919,#11920,#11921,#11922,#11923,
#11924,#11925,#11926,#11927,#11928),.UNSPECIFIED.,.F.,.F.,(4,2,2,2,4),(-0.385870474865139,
-0.31405913599211,-0.239369291297457,-0.135126671382209,0.),
 .UNSPECIFIED.);
#377=B_SPLINE_CURVE_WITH_KNOTS('',3,(#11933,#11934,#11935,#11936,#11937,
#11938,#11939,#11940,#11941,#11942,#11943,#11944,#11945,#11946,#11947,#11948),
 .UNSPECIFIED.,.F.,.F.,(4,2,2,2,2,2,2,4),(-0.5306283706703,-0.438179590528974,
-0.368258168563241,-0.304848975856583,-0.183637495296807,-0.11012433162058,
-0.0450078568695895,0.),.UNSPECIFIED.);
#378=B_SPLINE_CURVE_WITH_KNOTS('',3,(#11950,#11951,#11952,#11953,#11954,
#11955,#11956,#11957,#11958,#11959),.UNSPECIFIED.,.F.,.F.,(4,2,2,2,4),(-0.385870474981686,
-0.314059136066467,-0.23936929132688,-0.135126671387158,0.),
 .UNSPECIFIED.);
#379=B_SPLINE_CURVE_WITH_KNOTS('',3,(#11964,#11965,#11966,#11967,#11968,
#11969,#11970,#11971,#11972,#11973,#11974,#11975,#11976,#11977,#11978,#11979),
 .UNSPECIFIED.,.F.,.F.,(4,2,2,2,2,2,2,4),(-0.530628370630461,-0.438179590512618,
-0.368258168556241,-0.304848975849823,-0.183637495293183,-0.110124331618942,
-0.045007856869029,0.),.UNSPECIFIED.);
#380=B_SPLINE_CURVE_WITH_KNOTS('',3,(#11981,#11982,#11983,#11984,#11985,
#11986,#11987,#11988,#11989,#11990),.UNSPECIFIED.,.F.,.F.,(4,2,2,2,4),(-0.385870475012076,
-0.314059136083952,-0.239369291332893,-0.135126671387372,0.),
 .UNSPECIFIED.);
#381=B_SPLINE_CURVE_WITH_KNOTS('',3,(#11995,#11996,#11997,#11998,#11999,
#12000,#12001,#12002,#12003,#12004,#12005,#12006,#12007,#12008,#12009,#12010),
 .UNSPECIFIED.,.F.,.F.,(4,2,2,2,2,2,2,4),(-0.530628370690807,-0.438179590550982,
-0.36825816857982,-0.304848975865985,-0.183637495299133,-0.110124331620377,
-0.0450078568693689,0.),.UNSPECIFIED.);
#382=B_SPLINE_CURVE_WITH_KNOTS('',3,(#12012,#12013,#12014,#12015,#12016,
#12017,#12018,#12019,#12020,#12021),.UNSPECIFIED.,.F.,.F.,(4,2,2,2,4),(-0.385870474994837,
-0.314059136073306,-0.239369291329243,-0.135126671387283,0.),
 .UNSPECIFIED.);
#383=B_SPLINE_CURVE_WITH_KNOTS('',3,(#12026,#12027,#12028,#12029,#12030,
#12031,#12032,#12033,#12034,#12035,#12036,#12037,#12038,#12039,#12040,#12041),
 .UNSPECIFIED.,.F.,.F.,(4,2,2,2,2,2,2,4),(-0.530628370667125,-0.438179590523967,
-0.368258168558833,-0.304848975854,-0.183637495296909,-0.110124331621158,
-0.0450078568698694,0.),.UNSPECIFIED.);
#384=B_SPLINE_CURVE_WITH_KNOTS('',3,(#12043,#12044,#12045,#12046,#12047,
#12048,#12049,#12050,#12051,#12052),.UNSPECIFIED.,.F.,.F.,(4,2,2,2,4),(-0.385870474971746,
-0.31405913605961,-0.239369291323841,-0.135126671386237,0.),
 .UNSPECIFIED.);
#385=B_SPLINE_CURVE_WITH_KNOTS('',3,(#12067,#12068,#12069,#12070,#12071,
#12072,#12073,#12074,#12075,#12076,#12077,#12078,#12079,#12080,#12081,#12082),
 .UNSPECIFIED.,.F.,.F.,(4,2,2,2,2,2,2,4),(-0.530628370661766,-0.438179590520695,
-0.368258168559026,-0.304848975856584,-0.18363749529647,-0.110124331620193,
-0.0450078568694207,0.),.UNSPECIFIED.);
#386=B_SPLINE_CURVE_WITH_KNOTS('',3,(#12084,#12085,#12086,#12087,#12088,
#12089,#12090,#12091,#12092,#12093),.UNSPECIFIED.,.F.,.F.,(4,2,2,2,4),(-0.385870474867246,
-0.314059135993994,-0.239369291299197,-0.135126671383269,0.),
 .UNSPECIFIED.);
#387=B_SPLINE_CURVE_WITH_KNOTS('',3,(#12121,#12122,#12123,#12124,#12125,
#12126,#12127,#12128,#12129,#12130,#12131,#12132,#12133,#12134,#12135,#12136,
#12137,#12138,#12139,#12140,#12141,#12142,#12143,#12144,#12145,#12146,#12147,
#12148),.UNSPECIFIED.,.F.,.F.,(4,3,3,3,3,3,3,3,3,4),(0.,0.10535075562,0.211630470100858,
0.32063653562082,0.396655662726854,0.476762504776631,0.559142830371662,
0.643714126095473,0.734783989792354,0.799188564080633),.UNSPECIFIED.);
#388=B_SPLINE_CURVE_WITH_KNOTS('',3,(#12181,#12182,#12183,#12184,#12185,
#12186,#12187,#12188,#12189,#12190,#12191,#12192,#12193,#12194,#12195,#12196,
#12197,#12198,#12199,#12200,#12201,#12202,#12203,#12204,#12205,#12206,#12207,
#12208),.UNSPECIFIED.,.F.,.F.,(4,3,3,3,3,3,3,3,3,4),(0.,0.105350580727645,
0.211630157393727,0.320636018170041,0.39665566272708,0.476762496060542,
0.559143022698535,0.643714701417285,0.734784330146394,0.79918856408108),
 .UNSPECIFIED.);
#389=B_SPLINE_CURVE_WITH_KNOTS('',3,(#12241,#12242,#12243,#12244,#12245,
#12246,#12247,#12248,#12249,#12250,#12251,#12252,#12253,#12254,#12255,#12256,
#12257,#12258,#12259,#12260,#12261,#12262,#12263,#12264,#12265,#12266,#12267,
#12268),.UNSPECIFIED.,.F.,.F.,(4,3,3,3,3,3,3,3,3,4),(0.,0.105350505304636,
0.211630022763806,0.320635795967351,0.396655662726985,0.476762492451757,
0.559143105761226,0.643714949539588,0.734784479477035,0.799188564080899),
 .UNSPECIFIED.);
#390=B_SPLINE_CURVE_WITH_KNOTS('',3,(#12301,#12302,#12303,#12304,#12305,
#12306,#12307,#12308,#12309,#12310,#12311,#12312,#12313,#12314,#12315,#12316,
#12317,#12318,#12319,#12320,#12321,#12322,#12323,#12324,#12325,#12326,#12327,
#12328),.UNSPECIFIED.,.F.,.F.,(4,3,3,3,3,3,3,3,3,4),(0.,0.105350517029453,
0.21163004368367,0.320635830472424,0.39665566272694,0.476762493006737,0.559143092844083,
0.64371491096779,0.734784456165118,0.799188564080757),.UNSPECIFIED.);
#391=B_SPLINE_CURVE_WITH_KNOTS('',3,(#12361,#12362,#12363,#12364,#12365,
#12366,#12367,#12368,#12369,#12370,#12371,#12372,#12373,#12374,#12375,#12376,
#12377,#12378,#12379,#12380,#12381,#12382,#12383,#12384,#12385,#12386,#12387,
#12388),.UNSPECIFIED.,.F.,.F.,(4,3,3,3,3,3,3,3,3,4),(0.,0.105350617782938,
0.211630223586182,0.320636127543284,0.396655662726963,0.476762497865765,
0.559142981916141,0.643714579518275,0.734784257333252,0.79918856408084),
 .UNSPECIFIED.);
#392=B_SPLINE_CURVE_WITH_KNOTS('',3,(#12421,#12422,#12423,#12424,#12425,
#12426,#12427,#12428,#12429,#12430,#12431,#12432,#12433,#12434,#12435,#12436,
#12437,#12438,#12439,#12440,#12441,#12442,#12443,#12444,#12445,#12446,#12447,
#12448),.UNSPECIFIED.,.F.,.F.,(4,3,3,3,3,3,3,3,3,4),(0.,0.105350755620646,
0.211630470101819,0.320636535621585,0.396655662726938,0.476762504777025,
0.55914283037207,0.643714126095984,0.734783989792887,0.799188564080764),
 .UNSPECIFIED.);
#393=B_SPLINE_CURVE_WITH_KNOTS('',3,(#12481,#12482,#12483,#12484,#12485,
#12486,#12487,#12488,#12489,#12490,#12491,#12492,#12493,#12494,#12495,#12496,
#12497,#12498,#12499,#12500,#12501,#12502,#12503,#12504,#12505,#12506,#12507,
#12508),.UNSPECIFIED.,.F.,.F.,(4,3,3,3,3,3,3,3,3,4),(0.,0.105350580727718,
0.211630157393232,0.320636018169153,0.396655662726952,0.476762496060361,
0.559143022698262,0.643714701416882,0.734784330145906,0.799188564080778),
 .UNSPECIFIED.);
#394=B_SPLINE_CURVE_WITH_KNOTS('',3,(#12541,#12542,#12543,#12544,#12545,
#12546,#12547,#12548,#12549,#12550,#12551,#12552,#12553,#12554,#12555,#12556,
#12557,#12558,#12559,#12560,#12561,#12562,#12563,#12564,#12565,#12566,#12567,
#12568),.UNSPECIFIED.,.F.,.F.,(4,3,3,3,3,3,3,3,3,4),(0.,0.105350505304776,
0.211630022764475,0.320635795967906,0.396655662726964,0.476762492451559,
0.559143105761002,0.643714949539319,0.7347844794766,0.799188564080815),
 .UNSPECIFIED.);
#395=B_SPLINE_CURVE_WITH_KNOTS('',3,(#12601,#12602,#12603,#12604,#12605,
#12606,#12607,#12608,#12609,#12610,#12611,#12612,#12613,#12614,#12615,#12616,
#12617,#12618,#12619,#12620,#12621,#12622,#12623,#12624,#12625,#12626,#12627,
#12628),.UNSPECIFIED.,.F.,.F.,(4,3,3,3,3,3,3,3,3,4),(0.,0.105350517029029,
0.211630043683767,0.320635830472862,0.396655662727039,0.476762493006702,
0.559143092844054,0.643714910967833,0.734784456165161,0.799188564080931),
 .UNSPECIFIED.);
#396=B_SPLINE_CURVE_WITH_KNOTS('',3,(#12661,#12662,#12663,#12664,#12665,
#12666,#12667,#12668,#12669,#12670,#12671,#12672,#12673,#12674,#12675,#12676,
#12677,#12678,#12679,#12680,#12681,#12682,#12683,#12684,#12685,#12686,#12687,
#12688),.UNSPECIFIED.,.F.,.F.,(4,3,3,3,3,3,3,3,3,4),(0.,0.105350617782518,
0.211630223586211,0.320636127542873,0.396655662726838,0.476762497865674,
0.559142981916043,0.643714579518135,0.734784257333135,0.799188564080614),
 .UNSPECIFIED.);
#397=B_SPLINE_CURVE_WITH_KNOTS('',3,(#12721,#12722,#12723,#12724),
 .UNSPECIFIED.,.F.,.F.,(4,4),(0.,0.150716059332096),.UNSPECIFIED.);
#398=B_SPLINE_CURVE_WITH_KNOTS('',3,(#12757,#12758,#12759,#12760,#12761,
#12762,#12763,#12764,#12765,#12766,#12767,#12768,#12769,#12770,#12771,#12772,
#12773,#12774,#12775,#12776,#12777,#12778,#12779,#12780,#12781,#12782,#12783,
#12784),.UNSPECIFIED.,.F.,.F.,(4,3,3,3,3,3,3,3,3,4),(0.,0.1053505807278,
0.211630157393979,0.320636018170015,0.396655662727064,0.47676249606025,
0.559143022698166,0.643714701416806,0.734784330145882,0.799188564081011),
 .UNSPECIFIED.);
#399=B_SPLINE_CURVE_WITH_KNOTS('',3,(#12817,#12818,#12819,#12820,#12821,
#12822,#12823,#12824,#12825,#12826,#12827,#12828,#12829,#12830,#12831,#12832,
#12833,#12834,#12835,#12836,#12837,#12838,#12839,#12840,#12841,#12842,#12843,
#12844),.UNSPECIFIED.,.F.,.F.,(4,3,3,3,3,3,3,3,3,4),(0.,0.105350505304457,
0.21163002276398,0.320635795967329,0.396655662726986,0.476762492451752,
0.55914310576122,0.643714949539569,0.734784479476893,0.799188564080866),
 .UNSPECIFIED.);
#400=B_SPLINE_CURVE_WITH_KNOTS('',3,(#12877,#12878,#12879,#12880,#12881,
#12882,#12883,#12884,#12885,#12886,#12887,#12888,#12889,#12890,#12891,#12892,
#12893,#12894,#12895,#12896,#12897,#12898,#12899,#12900,#12901,#12902,#12903,
#12904),.UNSPECIFIED.,.F.,.F.,(4,3,3,3,3,3,3,3,3,4),(0.,0.105350517029183,
0.211630043683744,0.320635830472283,0.396655662726922,0.476762493006743,
0.559143092844057,0.6437149109678,0.734784456165119,0.799188564080692),
 .UNSPECIFIED.);
#401=B_SPLINE_CURVE_WITH_KNOTS('',3,(#12937,#12938,#12939,#12940,#12941,
#12942,#12943,#12944,#12945,#12946,#12947,#12948,#12949,#12950,#12951,#12952,
#12953,#12954,#12955,#12956,#12957,#12958,#12959,#12960,#12961,#12962,#12963,
#12964),.UNSPECIFIED.,.F.,.F.,(4,3,3,3,3,3,3,3,3,4),(0.,0.105350617782988,
0.211630223585978,0.320636127542671,0.396655662727022,0.476762497865844,
0.559142981916226,0.643714579518403,0.734784257333494,0.799188564080915),
 .UNSPECIFIED.);
#402=B_SPLINE_CURVE_WITH_KNOTS('',3,(#12997,#12998,#12999,#13000,#13001,
#13002,#13003,#13004,#13005,#13006,#13007,#13008,#13009,#13010,#13011,#13012,
#13013,#13014,#13015,#13016,#13017,#13018,#13019,#13020,#13021,#13022,#13023,
#13024),.UNSPECIFIED.,.F.,.F.,(4,3,3,3,3,3,3,3,3,4),(0.,0.105350755620161,
0.211630470100934,0.320636535620834,0.396655662727017,0.476762504776933,
0.559142830371988,0.643714126095916,0.734783989792824,0.799188564080951),
 .UNSPECIFIED.);
#403=B_SPLINE_CURVE_WITH_KNOTS('',3,(#13057,#13058,#13059,#13060,#13061,
#13062,#13063,#13064,#13065,#13066,#13067,#13068,#13069,#13070,#13071,#13072,
#13073,#13074,#13075,#13076,#13077,#13078,#13079,#13080,#13081,#13082,#13083,
#13084),.UNSPECIFIED.,.F.,.F.,(4,3,3,3,3,3,3,3,3,4),(0.,0.105350580727699,
0.211630157394061,0.320636018170424,0.396655662727046,0.476762496060293,
0.559143022698226,0.643714701416837,0.7347843301459,0.799188564080982),
 .UNSPECIFIED.);
#404=B_SPLINE_CURVE_WITH_KNOTS('',3,(#13117,#13118,#13119,#13120,#13121,
#13122,#13123,#13124,#13125,#13126,#13127,#13128,#13129,#13130,#13131,#13132,
#13133,#13134,#13135,#13136,#13137,#13138,#13139,#13140,#13141,#13142,#13143,
#13144),.UNSPECIFIED.,.F.,.F.,(4,3,3,3,3,3,3,3,3,4),(0.,0.105350505304653,
0.211630022764195,0.320635795967923,0.396655662727108,0.476762492451716,
0.559143105761212,0.643714949539593,0.734784479477028,0.79918856408114),
 .UNSPECIFIED.);
#405=B_SPLINE_CURVE_WITH_KNOTS('',3,(#13177,#13178,#13179,#13180,#13181,
#13182,#13183,#13184,#13185,#13186,#13187,#13188,#13189,#13190,#13191,#13192,
#13193,#13194,#13195,#13196,#13197,#13198,#13199,#13200,#13201,#13202,#13203,
#13204),.UNSPECIFIED.,.F.,.F.,(4,3,3,3,3,3,3,3,3,4),(0.,0.105350517029269,
0.211630043683721,0.320635830472785,0.396655662726906,0.476762493006721,
0.559143092844096,0.643714910967841,0.734784456165104,0.799188564080754),
 .UNSPECIFIED.);
#406=B_SPLINE_CURVE_WITH_KNOTS('',3,(#13237,#13238,#13239,#13240,#13241,
#13242,#13243,#13244,#13245,#13246,#13247,#13248,#13249,#13250,#13251,#13252,
#13253,#13254,#13255,#13256,#13257,#13258,#13259,#13260,#13261,#13262,#13263,
#13264),.UNSPECIFIED.,.F.,.F.,(4,3,3,3,3,3,3,3,3,4),(0.,0.105350617782791,
0.211630223586115,0.320636127543467,0.396655662727067,0.476762497865883,
0.559142981916264,0.643714579518415,0.734784257333419,0.799188564081055),
 .UNSPECIFIED.);
#407=B_SPLINE_CURVE_WITH_KNOTS('',3,(#13388,#13389,#13390,#13391,#13392,
#13393,#13394,#13395,#13396,#13397,#13398,#13399,#13400,#13401,#13402,#13403,
#13404,#13405,#13406,#13407,#13408,#13409,#13410,#13411,#13412,#13413,#13414,
#13415,#13416,#13417,#13418,#13419,#13420,#13421,#13422,#13423,#13424,#13425,
#13426,#13427),.UNSPECIFIED.,.F.,.F.,(4,3,3,3,3,3,3,3,3,3,3,3,3,4),(0.,
0.080816837337899,0.159744691662406,0.238272865643827,0.316637951909253,
0.39214567920225,0.451150927438286,0.506701203283771,0.5619638530984,0.663361603296831,
0.672200447289742,0.727455868377893,0.755180292788767,0.782993887761336),
 .UNSPECIFIED.);
#408=B_SPLINE_CURVE_WITH_KNOTS('',3,(#13435,#13436,#13437,#13438,#13439,
#13440),.UNSPECIFIED.,.F.,.F.,(4,2,4),(0.07026331290575,0.392145679202251,
0.782993887761363),.UNSPECIFIED.);
#409=B_SPLINE_CURVE_WITH_KNOTS('',3,(#13443,#13444,#13445,#13446,#13447,
#13448,#13449,#13450,#13451,#13452,#13453,#13454,#13455,#13456,#13457,#13458,
#13459,#13460,#13461,#13462,#13463,#13464,#13465,#13466,#13467,#13468,#13469,
#13470),.UNSPECIFIED.,.F.,.F.,(4,3,3,3,3,3,3,3,3,4),(0.,0.0804727531474491,
0.159375053173973,0.237925353906231,0.316349809181948,0.39214567920222,
0.495918215505369,0.598324344999396,0.699619020094378,0.782993887761245),
 .UNSPECIFIED.);
#410=B_SPLINE_CURVE_WITH_KNOTS('',3,(#13473,#13474,#13475,#13476,#13477,
#13478,#13479,#13480,#13481,#13482,#13483,#13484,#13485,#13486,#13487,#13488,
#13489,#13490,#13491,#13492,#13493,#13494,#13495,#13496,#13497,#13498,#13499,
#13500,#13501,#13502,#13503,#13504,#13505,#13506,#13507,#13508,#13509,#13510,
#13511,#13512),.UNSPECIFIED.,.F.,.F.,(4,3,3,3,3,3,3,3,3,3,3,3,3,4),(0.,
0.0808237501538664,0.159752125840751,0.238279961562834,0.31664406989611,
0.392145679202288,0.45115092743835,0.50670120328386,0.561963853098512,0.663377487277087,
0.672200447289889,0.727455868378047,0.755180292788921,0.782993887761487),
 .UNSPECIFIED.);
#411=B_SPLINE_CURVE_WITH_KNOTS('',3,(#13515,#13516,#13517,#13518,#13519,
#13520,#13521,#13522,#13523,#13524,#13525,#13526,#13527,#13528,#13529,#13530,
#13531,#13532,#13533,#13534,#13535,#13536,#13537,#13538,#13539,#13540,#13541,
#13542,#13543,#13544,#13545,#13546,#13547,#13548,#13549,#13550,#13551,#13552,
#13553,#13554),.UNSPECIFIED.,.F.,.F.,(4,3,3,3,3,3,3,3,3,3,3,3,3,4),(0.,
0.080826365016996,0.15975466022045,0.238282174042087,0.316645830807802,
0.392145679202281,0.451150927438327,0.506701203283823,0.561963853098462,
0.663386079795717,0.672200447289833,0.727455868378004,0.75518029278889,
0.782993887761473),.UNSPECIFIED.);
#412=B_SPLINE_CURVE_WITH_KNOTS('',3,(#13557,#13558,#13559,#13560,#13561,
#13562,#13563,#13564,#13565,#13566,#13567,#13568,#13569,#13570,#13571,#13572,
#13573,#13574,#13575,#13576,#13577,#13578,#13579,#13580,#13581,#13582,#13583,
#13584,#13585,#13586,#13587,#13588,#13589,#13590,#13591,#13592,#13593,#13594,
#13595,#13596),.UNSPECIFIED.,.F.,.F.,(4,3,3,3,3,3,3,3,3,3,3,3,3,4),(0.,
0.0808168373377941,0.15974469166233,0.238272865643754,0.316637951909167,
0.392145679202253,0.451150927438289,0.506701203283775,0.561963853098404,
0.663361603296804,0.672200447289745,0.727455868377895,0.755180292788769,
0.782993887761338),.UNSPECIFIED.);
#413=B_SPLINE_CURVE_WITH_KNOTS('',3,(#13599,#13600,#13601,#13602,#13603,
#13604,#13605,#13606,#13607,#13608,#13609,#13610,#13611,#13612,#13613,#13614,
#13615,#13616,#13617,#13618,#13619,#13620,#13621,#13622,#13623,#13624,#13625,
#13626),.UNSPECIFIED.,.F.,.F.,(4,3,3,3,3,3,3,3,3,4),(0.,0.0804773681583594,
0.159381289585917,0.237932353538847,0.316356775343447,0.392145679202256,
0.495917404016704,0.598322903162837,0.699618128903555,0.782993887761399),
 .UNSPECIFIED.);
#414=B_SPLINE_CURVE_WITH_KNOTS('',3,(#13629,#13630,#13631,#13632,#13633,
#13634,#13635,#13636,#13637,#13638,#13639,#13640,#13641,#13642,#13643,#13644,
#13645,#13646,#13647,#13648,#13649,#13650,#13651,#13652,#13653,#13654,#13655,
#13656),.UNSPECIFIED.,.F.,.F.,(4,3,3,3,3,3,3,3,3,4),(0.,0.0804727531474338,
0.159375053174015,0.237925353906301,0.316349809182045,0.392145679202232,
0.495918215505487,0.598324344999523,0.699619020094104,0.78299388776127),
 .UNSPECIFIED.);
#415=B_SPLINE_CURVE_WITH_KNOTS('',3,(#13659,#13660,#13661,#13662,#13663,
#13664,#13665,#13666,#13667,#13668,#13669,#13670,#13671,#13672,#13673,#13674,
#13675,#13676,#13677,#13678,#13679,#13680,#13681,#13682,#13683,#13684,#13685,
#13686,#13687,#13688,#13689,#13690,#13691,#13692,#13693,#13694,#13695,#13696,
#13697,#13698),.UNSPECIFIED.,.F.,.F.,(4,3,3,3,3,3,3,3,3,3,3,3,3,4),(0.,
0.0808237501539957,0.159752125840905,0.23827996156287,0.316644069896139,
0.392145679202281,0.451150927438335,0.506701203283837,0.561963853098483,
0.663377487276743,0.672200447289856,0.727455868378023,0.755180292788905,
0.782993887761481),.UNSPECIFIED.);
#416=B_SPLINE_CURVE_WITH_KNOTS('',3,(#13701,#13702,#13703,#13704,#13705,
#13706,#13707,#13708,#13709,#13710,#13711,#13712,#13713,#13714,#13715,#13716,
#13717,#13718,#13719,#13720,#13721,#13722,#13723,#13724,#13725,#13726,#13727,
#13728,#13729,#13730,#13731,#13732,#13733,#13734,#13735,#13736,#13737,#13738,
#13739,#13740),.UNSPECIFIED.,.F.,.F.,(4,3,3,3,3,3,3,3,3,3,3,3,3,4),(0.,
0.0808263650166872,0.159754660220132,0.238282174041845,0.316645830807606,
0.392145679202287,0.451150927438335,0.506701203283831,0.561963853098472,
0.663386079795103,0.672200447289846,0.72745586837802,0.755180292788908,
0.782993887761494),.UNSPECIFIED.);
#417=B_SPLINE_CURVE_WITH_KNOTS('',3,(#13743,#13744,#13745,#13746,#13747,
#13748,#13749,#13750,#13751,#13752,#13753,#13754,#13755,#13756,#13757,#13758,
#13759,#13760,#13761,#13762,#13763,#13764,#13765,#13766,#13767,#13768,#13769,
#13770),.UNSPECIFIED.,.F.,.F.,(4,3,3,3,3,3,3,3,3,4),(0.,0.0804773681583258,
0.15938128958588,0.237932353538843,0.316356775343476,0.392145679202253,
0.495917404016412,0.5983229031625,0.699618128903188,0.782993887761353),
 .UNSPECIFIED.);
#418=B_SPLINE_CURVE_WITH_KNOTS('',3,(#13773,#13774,#13775,#13776,#13777,
#13778,#13779,#13780,#13781,#13782,#13783,#13784,#13785,#13786,#13787,#13788,
#13789,#13790,#13791,#13792,#13793,#13794,#13795,#13796,#13797,#13798,#13799,
#13800),.UNSPECIFIED.,.F.,.F.,(4,3,3,3,3,3,3,3,3,4),(0.,0.08047275314732,
0.15937505317391,0.237925353906137,0.316349809181831,0.392145679202234,
0.495918215505687,0.598324344999879,0.699619020095004,0.782993887761323),
 .UNSPECIFIED.);
#419=B_SPLINE_CURVE_WITH_KNOTS('',3,(#13803,#13804,#13805,#13806,#13807,
#13808,#13809,#13810,#13811,#13812,#13813,#13814,#13815,#13816,#13817,#13818,
#13819,#13820,#13821,#13822,#13823,#13824,#13825,#13826,#13827,#13828,#13829,
#13830,#13831,#13832,#13833,#13834,#13835,#13836,#13837,#13838,#13839,#13840,
#13841,#13842),.UNSPECIFIED.,.F.,.F.,(4,3,3,3,3,3,3,3,3,3,3,3,3,4),(0.,
0.0808237501538626,0.159752125840739,0.238279961562764,0.316644069896114,
0.392145679202252,0.451150927438296,0.50670120328379,0.561963853098427,
0.663377487277723,0.672200447289778,0.727455868377928,0.7551802927888,0.782993887761365),
 .UNSPECIFIED.);
#420=B_SPLINE_CURVE_WITH_KNOTS('',3,(#13845,#13846,#13847,#13848,#13849,
#13850,#13851,#13852,#13853,#13854,#13855,#13856,#13857,#13858,#13859,#13860,
#13861,#13862,#13863,#13864,#13865,#13866,#13867,#13868,#13869,#13870,#13871,
#13872,#13873,#13874,#13875,#13876,#13877,#13878,#13879,#13880,#13881,#13882,
#13883,#13884),.UNSPECIFIED.,.F.,.F.,(4,3,3,3,3,3,3,3,3,3,3,3,3,4),(0.,
0.0808263650167775,0.159754660220236,0.238282174041904,0.316645830807637,
0.39214567920233,0.451150927438407,0.506701203283934,0.561963853098602,
0.663386079793417,0.672200447290009,0.72745586837818,0.755180292789061,
0.782993887761632),.UNSPECIFIED.);
#421=B_SPLINE_CURVE_WITH_KNOTS('',3,(#13887,#13888,#13889,#13890,#13891,
#13892,#13893,#13894,#13895,#13896,#13897,#13898,#13899,#13900,#13901,#13902,
#13903,#13904,#13905,#13906,#13907,#13908,#13909,#13910,#13911,#13912,#13913,
#13914,#13915,#13916,#13917,#13918,#13919,#13920,#13921,#13922,#13923,#13924,
#13925,#13926),.UNSPECIFIED.,.F.,.F.,(4,3,3,3,3,3,3,3,3,3,3,3,3,4),(0.,
0.0808168373377771,0.159744691662314,0.238272865643762,0.316637951909151,
0.392145679202262,0.451150927438304,0.506701203283795,0.561963853098429,
0.66336160329673,0.672200447289777,0.727455868377926,0.755180292788798,
0.782993887761364),.UNSPECIFIED.);
#422=B_SPLINE_CURVE_WITH_KNOTS('',3,(#13929,#13930,#13931,#13932,#13933,
#13934,#13935,#13936,#13937,#13938,#13939,#13940,#13941,#13942,#13943,#13944,
#13945,#13946,#13947,#13948,#13949,#13950,#13951,#13952,#13953,#13954,#13955,
#13956),.UNSPECIFIED.,.F.,.F.,(4,3,3,3,3,3,3,3,3,4),(0.,0.0804773681583631,
0.15938128958592,0.237932353538891,0.316356775343511,0.392145679202255,
0.495917404016605,0.598322903162788,0.699618128903027,0.782993887761362),
 .UNSPECIFIED.);
#423=B_SPLINE_CURVE_WITH_KNOTS('',3,(#13959,#13960,#13961,#13962,#13963,
#13964,#13965,#13966,#13967,#13968,#13969,#13970,#13971,#13972,#13973,#13974,
#13975,#13976,#13977,#13978,#13979,#13980,#13981,#13982,#13983,#13984,#13985,
#13986),.UNSPECIFIED.,.F.,.F.,(4,3,3,3,3,3,3,3,3,4),(0.,0.0804727531475009,
0.159375053174066,0.237925353906258,0.316349809181868,0.392145679202247,
0.495918215505489,0.598324344999634,0.699619020094664,0.782993887761332),
 .UNSPECIFIED.);
#424=B_SPLINE_CURVE_WITH_KNOTS('',3,(#13989,#13990,#13991,#13992,#13993,
#13994,#13995,#13996,#13997,#13998,#13999,#14000,#14001,#14002,#14003,#14004,
#14005,#14006,#14007,#14008,#14009,#14010,#14011,#14012,#14013,#14014,#14015,
#14016,#14017,#14018,#14019,#14020,#14021,#14022,#14023,#14024,#14025,#14026,
#14027,#14028),.UNSPECIFIED.,.F.,.F.,(4,3,3,3,3,3,3,3,3,3,3,3,3,4),(0.,
0.0808237501538716,0.159752125840756,0.238279961562882,0.316644069896221,
0.392145679202287,0.451150927438346,0.506701203283854,0.561963853098504,
0.663377487277437,0.672200447289882,0.727455868378044,0.755180292788922,
0.782993887761492),.UNSPECIFIED.);
#425=B_SPLINE_CURVE_WITH_KNOTS('',3,(#14031,#14032,#14033,#14034,#14035,
#14036,#14037,#14038,#14039,#14040,#14041,#14042,#14043,#14044,#14045,#14046,
#14047,#14048,#14049,#14050,#14051,#14052,#14053,#14054,#14055,#14056,#14057,
#14058,#14059,#14060,#14061,#14062,#14063,#14064,#14065,#14066,#14067,#14068,
#14069,#14070),.UNSPECIFIED.,.F.,.F.,(4,3,3,3,3,3,3,3,3,3,3,3,3,4),(0.,
0.0808263650167331,0.159754660220215,0.238282174041877,0.316645830807603,
0.39214567920227,0.451150927438306,0.506701203283791,0.561963853098421,
0.663386079794874,0.672200447289781,0.727455868377954,0.755180292788844,
0.782993887761433),.UNSPECIFIED.);
#426=B_SPLINE_CURVE_WITH_KNOTS('',3,(#14073,#14074,#14075,#14076,#14077,
#14078,#14079,#14080,#14081,#14082,#14083,#14084,#14085,#14086,#14087,#14088,
#14089,#14090,#14091,#14092,#14093,#14094,#14095,#14096,#14097,#14098,#14099,
#14100,#14101,#14102,#14103,#14104,#14105,#14106,#14107,#14108,#14109,#14110,
#14111,#14112),.UNSPECIFIED.,.F.,.F.,(4,3,3,3,3,3,3,3,3,3,3,3,3,4),(0.,
0.0808168373379184,0.159744691662454,0.238272865643917,0.316637951909378,
0.39214567920226,0.451150927438305,0.506701203283801,0.561963853098441,
0.663361603296352,0.672200447289796,0.727455868377948,0.755180292788821,
0.782993887761387),.UNSPECIFIED.);
#427=B_SPLINE_CURVE_WITH_KNOTS('',3,(#15846,#15847,#15848,#15849,#15850,
#15851,#15852,#15853,#15854,#15855),.UNSPECIFIED.,.F.,.F.,(4,2,2,2,4),(0.331186461688063,
0.41497096063171,0.498755459575358,0.580564191475742,0.662372923376126),
 .UNSPECIFIED.);
#428=B_SPLINE_CURVE_WITH_KNOTS('',3,(#15857,#15858,#15859,#15860,#15861,
#15862,#15863,#15864,#15865,#15866,#15867,#15868,#15869,#15870,#15871,#15872,
#15873,#15874,#15875),.UNSPECIFIED.,.F.,.F.,(4,2,2,2,3,2,2,2,4),(0.993559385064188,
1.07734388400784,1.16112838295148,1.24293711485187,1.32474584675225,1.40655457865263,
1.48836331055302,1.57214780949667,1.65593230844031),.UNSPECIFIED.);
#429=B_SPLINE_CURVE_WITH_KNOTS('',3,(#15876,#15877,#15878,#15879,#15880,
#15881,#15882,#15883,#15884,#15885),.UNSPECIFIED.,.F.,.F.,(4,2,2,2,4),(0.662372923376126,
0.744181655276509,0.825990387176893,0.909774886120541,0.993559385064188),
 .UNSPECIFIED.);
#430=B_SPLINE_CURVE_WITH_KNOTS('',3,(#15893,#15894,#15895,#15896,#15897,
#15898,#15899,#15900,#15901,#15902),.UNSPECIFIED.,.F.,.F.,(4,2,2,2,4),(0.934777550778115,
1.01265597092338,1.09053439106865,1.1684522293864,1.24637006770415),
 .UNSPECIFIED.);
#431=B_SPLINE_CURVE_WITH_KNOTS('',3,(#15904,#15905,#15906,#15907,#15908,
#15909,#15910,#15911,#15912,#15913,#15914,#15915,#15916,#15917,#15918,#15919,
#15920,#15921),.UNSPECIFIED.,.F.,.F.,(4,2,2,2,2,2,2,2,4),(0.311592516926038,
0.389470937071308,0.467349357216578,0.545267195534327,0.623185033852077,
0.701102872169826,0.779020710487576,0.856899130632846,0.934777550778115),
 .UNSPECIFIED.);
#432=B_SPLINE_CURVE_WITH_KNOTS('',3,(#15922,#15923,#15924,#15925,#15926,
#15927,#15928,#15929,#15930,#15931),.UNSPECIFIED.,.F.,.F.,(4,2,2,2,4),(0.,
0.0779178383177495,0.155835676635499,0.233714096780769,0.311592516926038),
 .UNSPECIFIED.);
#433=B_SPLINE_CURVE_WITH_KNOTS('',3,(#15935,#15936,#15937,#15938,#15939,
#15940,#15941,#15942,#15943,#15944,#15945,#15946,#15947,#15948,#15949,#15950,
#15951,#15952),.UNSPECIFIED.,.F.,.F.,(4,2,2,2,2,2,2,2,4),(0.331186461688063,
0.41497096063171,0.498755459575358,0.580564191475742,0.662372923376126,
0.744181655276509,0.825990387176893,0.909774886120541,0.993559385064188),
 .UNSPECIFIED.);
#434=B_SPLINE_CURVE_WITH_KNOTS('',3,(#15956,#15957,#15958,#15959,#15960,
#15961,#15962,#15963,#15964,#15965,#15966,#15967,#15968,#15969,#15970,#15971,
#15972,#15973,#15974),.UNSPECIFIED.,.F.,.F.,(4,2,2,2,3,2,2,2,4),(0.993559385064188,
1.07734388400784,1.16112838295148,1.24293711485187,1.32474584675225,1.40655457865263,
1.48836331055302,1.57214780949667,1.65593230844031),.UNSPECIFIED.);
#435=B_SPLINE_CURVE_WITH_KNOTS('',3,(#15979,#15980,#15981,#15982,#15983,
#15984,#15985,#15986,#15987,#15988),.UNSPECIFIED.,.F.,.F.,(4,2,2,2,4),(0.,
0.0779178383177495,0.155835676635499,0.233714096780769,0.311592516926038),
 .UNSPECIFIED.);
#436=B_SPLINE_CURVE_WITH_KNOTS('',3,(#15989,#15990,#15991,#15992,#15993,
#15994,#15995,#15996,#15997,#15998,#15999,#16000,#16001,#16002,#16003,#16004,
#16005,#16006,#16007,#16008,#16009,#16010,#16011,#16012,#16013,#16014),
 .UNSPECIFIED.,.F.,.F.,(4,2,2,2,2,2,2,2,2,2,2,2,4),(0.311592516926038,0.389470937071308,
0.467349357216578,0.545267195534327,0.623185033852077,0.701102872169826,
0.779020710487576,0.856899130632846,0.934777550778115,1.01265597092338,
1.09053439106865,1.1684522293864,1.24637006770415),.UNSPECIFIED.);
#437=B_SPLINE_CURVE_WITH_KNOTS('',3,(#17532,#17533,#17534,#17535,#17536,
#17537,#17538,#17539,#17540,#17541,#17542,#17543,#17544,#17545),
 .UNSPECIFIED.,.F.,.F.,(4,2,2,2,2,2,4),(-0.255031134424107,-0.227793077275375,
-0.200453310558795,-0.154190090586012,-0.0736931236043211,-0.0424502065770208,
0.),.UNSPECIFIED.);
#438=B_SPLINE_CURVE_WITH_KNOTS('',3,(#17547,#17548,#17549,#17550,#17551,
#17552,#17553,#17554,#17555,#17556),.UNSPECIFIED.,.F.,.F.,(4,2,2,2,4),(-0.479798392309333,
-0.376300454690274,-0.276804242236344,-0.133663587529964,0.),
 .UNSPECIFIED.);
#439=B_SPLINE_CURVE_WITH_KNOTS('',3,(#17561,#17562,#17563,#17564,#17565,
#17566,#17567,#17568,#17569,#17570,#17571,#17572,#17573,#17574),
 .UNSPECIFIED.,.F.,.F.,(4,2,2,2,2,2,4),(-0.255031134475439,-0.227793077318937,
-0.200453310595062,-0.154190090611401,-0.0736931236137319,-0.0424502065803019,
0.),.UNSPECIFIED.);
#440=B_SPLINE_CURVE_WITH_KNOTS('',3,(#17576,#17577,#17578,#17579,#17580,
#17581,#17582,#17583,#17584,#17585),.UNSPECIFIED.,.F.,.F.,(4,2,2,2,4),(-0.479798392297146,
-0.37630045468042,-0.27680424222853,-0.133663587527001,0.),
 .UNSPECIFIED.);
#441=B_SPLINE_CURVE_WITH_KNOTS('',3,(#17590,#17591,#17592,#17593,#17594,
#17595,#17596,#17597,#17598,#17599,#17600,#17601,#17602,#17603),
 .UNSPECIFIED.,.F.,.F.,(4,2,2,2,2,2,4),(-0.255031134390982,-0.227793077246187,
-0.200453310533645,-0.154190090567835,-0.0736931235979434,-0.0424502065748416,
0.),.UNSPECIFIED.);
#442=B_SPLINE_CURVE_WITH_KNOTS('',3,(#17605,#17606,#17607,#17608,#17609,
#17610,#17611,#17612,#17613,#17614),.UNSPECIFIED.,.F.,.F.,(4,2,2,2,4),(-0.479798392957855,
-0.376300455154524,-0.276804242523407,-0.133663587595138,0.),
 .UNSPECIFIED.);
#443=B_SPLINE_CURVE_WITH_KNOTS('',3,(#17619,#17620,#17621,#17622,#17623,
#17624,#17625,#17626,#17627,#17628,#17629,#17630,#17631,#17632),
 .UNSPECIFIED.,.F.,.F.,(4,2,2,2,2,2,4),(-0.25503113453975,-0.227793077375508,
-0.200453310643473,-0.154190090645765,-0.0736931236262053,-0.042450206584545,
0.),.UNSPECIFIED.);
#444=B_SPLINE_CURVE_WITH_KNOTS('',3,(#17634,#17635,#17636,#17637,#17638,
#17639,#17640,#17641,#17642,#17643),.UNSPECIFIED.,.F.,.F.,(4,2,2,2,4),(-0.4797983929588,
-0.376300455156708,-0.276804242527526,-0.133663587598599,0.),
 .UNSPECIFIED.);
#445=B_SPLINE_CURVE_WITH_KNOTS('',3,(#17648,#17649,#17650,#17651,#17652,
#17653,#17654,#17655,#17656,#17657,#17658,#17659,#17660,#17661),
 .UNSPECIFIED.,.F.,.F.,(4,2,2,2,2,2,4),(-0.255031134416776,-0.227793077270562,
-0.200453310555608,-0.15419009058357,-0.0736931236038192,-0.0424502065768682,
0.),.UNSPECIFIED.);
#446=B_SPLINE_CURVE_WITH_KNOTS('',3,(#17663,#17664,#17665,#17666,#17667,
#17668,#17669,#17670,#17671,#17672),.UNSPECIFIED.,.F.,.F.,(4,2,2,2,4),(-0.479798392586391,
-0.376300454883909,-0.276804242349972,-0.133663587552267,0.),
 .UNSPECIFIED.);
#447=B_SPLINE_CURVE_WITH_KNOTS('',3,(#17677,#17678,#17679,#17680,#17681,
#17682,#17683,#17684,#17685,#17686,#17687,#17688,#17689,#17690),
 .UNSPECIFIED.,.F.,.F.,(4,2,2,2,2,2,4),(-0.255031134441827,-0.227793077287078,
-0.200453310565949,-0.154190090589066,-0.0736931236047745,-0.0424502065771008,
0.),.UNSPECIFIED.);
#448=B_SPLINE_CURVE_WITH_KNOTS('',3,(#17692,#17693,#17694,#17695,#17696,
#17697,#17698,#17699,#17700,#17701),.UNSPECIFIED.,.F.,.F.,(4,2,2,2,4),(-0.479798392309589,
-0.376300454691115,-0.276804242237601,-0.133663587530458,0.),
 .UNSPECIFIED.);
#449=B_SPLINE_CURVE_WITH_KNOTS('',3,(#17706,#17707,#17708,#17709,#17710,
#17711,#17712,#17713,#17714,#17715,#17716,#17717,#17718,#17719),
 .UNSPECIFIED.,.F.,.F.,(4,2,2,2,2,2,4),(-0.255031134477938,-0.227793077321361,
-0.20045331059734,-0.154190090613293,-0.0736931236147239,-0.0424502065806451,
0.),.UNSPECIFIED.);
#450=B_SPLINE_CURVE_WITH_KNOTS('',3,(#17721,#17722,#17723,#17724,#17725,
#17726,#17727,#17728,#17729,#17730),.UNSPECIFIED.,.F.,.F.,(4,2,2,2,4),(-0.479798392040146,
-0.376300454496221,-0.276804242114272,-0.133663587500383,0.),
 .UNSPECIFIED.);
#451=B_SPLINE_CURVE_WITH_KNOTS('',3,(#17735,#17736,#17737,#17738,#17739,
#17740,#17741,#17742,#17743,#17744,#17745,#17746,#17747,#17748),
 .UNSPECIFIED.,.F.,.F.,(4,2,2,2,2,2,4),(-0.255031134491615,-0.227793077335448,
-0.200453310611234,-0.154190090625469,-0.0736931236214063,-0.0424502065831927,
0.),.UNSPECIFIED.);
#452=B_SPLINE_CURVE_WITH_KNOTS('',3,(#17750,#17751,#17752,#17753,#17754,
#17755,#17756,#17757,#17758,#17759),.UNSPECIFIED.,.F.,.F.,(4,2,2,2,4),(-0.479798392731553,
-0.376300454992231,-0.276804242422527,-0.133663587571995,0.),
 .UNSPECIFIED.);
#453=B_SPLINE_CURVE_WITH_KNOTS('',3,(#17764,#17765,#17766,#17767,#17768,
#17769,#17770,#17771,#17772,#17773,#17774,#17775,#17776,#17777),
 .UNSPECIFIED.,.F.,.F.,(4,2,2,2,2,2,4),(-0.255031134337196,-0.227793077196323,
-0.200453310488615,-0.154190090533156,-0.0736931235840354,-0.0424502065698458,
0.),.UNSPECIFIED.);
#454=B_SPLINE_CURVE_WITH_KNOTS('',3,(#17779,#17780,#17781,#17782,#17783,
#17784,#17785,#17786,#17787,#17788),.UNSPECIFIED.,.F.,.F.,(4,2,2,2,4),(-0.479798391697847,
-0.376300454258333,-0.276804241976759,-0.133663587475283,0.),
 .UNSPECIFIED.);
#455=B_SPLINE_CURVE_WITH_KNOTS('',3,(#17793,#17794,#17795,#17796,#17797,
#17798,#17799,#17800,#17801,#17802,#17803,#17804,#17805,#17806),
 .UNSPECIFIED.,.F.,.F.,(4,2,2,2,2,2,4),(-0.255031134300382,-0.227793077166129,
-0.200453310466903,-0.154190090528462,-0.0736931235865039,-0.0424502065710793,
0.),.UNSPECIFIED.);
#456=B_SPLINE_CURVE_WITH_KNOTS('',3,(#17808,#17809,#17810,#17811,#17812,
#17813,#17814,#17815,#17816,#17817),.UNSPECIFIED.,.F.,.F.,(4,2,2,2,4),(-0.479798391515407,
-0.376300454120398,-0.276804241882046,-0.133663587447611,0.),
 .UNSPECIFIED.);
#457=B_SPLINE_CURVE_WITH_KNOTS('',3,(#17822,#17823,#17824,#17825,#17826,
#17827,#17828,#17829,#17830,#17831,#17832,#17833,#17834,#17835),
 .UNSPECIFIED.,.F.,.F.,(4,2,2,2,2,2,4),(-0.255031134433992,-0.227793077286409,
-0.200453310570116,-0.154190090595771,-0.0736931236079108,-0.0424502065782311,
0.),.UNSPECIFIED.);
#458=B_SPLINE_CURVE_WITH_KNOTS('',3,(#17837,#17838,#17839,#17840,#17841,
#17842,#17843,#17844,#17845,#17846),.UNSPECIFIED.,.F.,.F.,(4,2,2,2,4),(-0.479798392302676,
-0.376300454686334,-0.276804242234968,-0.133663587529961,0.),
 .UNSPECIFIED.);
#459=B_SPLINE_CURVE_WITH_KNOTS('',3,(#17851,#17852,#17853,#17854,#17855,
#17856,#17857,#17858,#17859,#17860,#17861,#17862,#17863,#17864),
 .UNSPECIFIED.,.F.,.F.,(4,2,2,2,2,2,4),(-0.255031134436975,-0.227793077286682,
-0.200453310569877,-0.154190090598983,-0.0736931236101461,-0.0424502065791056,
0.),.UNSPECIFIED.);
#460=B_SPLINE_CURVE_WITH_KNOTS('',3,(#17866,#17867,#17868,#17869,#17870,
#17871,#17872,#17873,#17874,#17875),.UNSPECIFIED.,.F.,.F.,(4,2,2,2,4),(-0.479798392050366,
-0.37630045450428,-0.276804242120537,-0.133663587502534,0.),
 .UNSPECIFIED.);
#461=B_SPLINE_CURVE_WITH_KNOTS('',3,(#17880,#17881,#17882,#17883,#17884,
#17885,#17886,#17887,#17888,#17889,#17890,#17891,#17892,#17893),
 .UNSPECIFIED.,.F.,.F.,(4,2,2,2,2,2,4),(-0.255031134555854,-0.227793077394919,
-0.200453310664611,-0.154190090665751,-0.0736931236342781,-0.0424502065874606,
0.),.UNSPECIFIED.);
#462=B_SPLINE_CURVE_WITH_KNOTS('',3,(#17895,#17896,#17897,#17898,#17899,
#17900,#17901,#17902,#17903,#17904),.UNSPECIFIED.,.F.,.F.,(4,2,2,2,4),(-0.479798392574118,
-0.376300454878286,-0.276804242350487,-0.133663587555216,0.),
 .UNSPECIFIED.);
#463=B_SPLINE_CURVE_WITH_KNOTS('',3,(#17909,#17910,#17911,#17912,#17913,
#17914,#17915,#17916,#17917,#17918,#17919,#17920,#17921,#17922),
 .UNSPECIFIED.,.F.,.F.,(4,2,2,2,2,2,4),(-0.255031134589258,-0.227793077418444,
-0.200453310681013,-0.154190090675844,-0.0736931236365812,-0.042450206588134,
0.),.UNSPECIFIED.);
#464=B_SPLINE_CURVE_WITH_KNOTS('',3,(#17924,#17925,#17926,#17927,#17928,
#17929,#17930,#17931,#17932,#17933),.UNSPECIFIED.,.F.,.F.,(4,2,2,2,4),(-0.479798391705042,
-0.376300454262635,-0.276804241978204,-0.13366358747526,0.),
 .UNSPECIFIED.);
#465=B_SPLINE_CURVE_WITH_KNOTS('',3,(#17938,#17939,#17940,#17941,#17942,
#17943,#17944,#17945,#17946,#17947,#17948,#17949,#17950,#17951),
 .UNSPECIFIED.,.F.,.F.,(4,2,2,2,2,2,4),(-0.255031134410801,-0.227793077261618,
-0.200453310546074,-0.154190090578359,-0.0736931236015757,-0.0424502065760304,
0.),.UNSPECIFIED.);
#466=B_SPLINE_CURVE_WITH_KNOTS('',3,(#17953,#17954,#17955,#17956,#17957,
#17958,#17959,#17960,#17961,#17962),.UNSPECIFIED.,.F.,.F.,(4,2,2,2,4),(-0.47979839227541,
-0.376300454666073,-0.27680424222116,-0.133663587524637,0.),
 .UNSPECIFIED.);
#467=B_SPLINE_CURVE_WITH_KNOTS('',3,(#17967,#17968,#17969,#17970,#17971,
#17972,#17973,#17974,#17975,#17976,#17977,#17978,#17979,#17980),
 .UNSPECIFIED.,.F.,.F.,(4,2,2,2,2,2,4),(-0.255031134458131,-0.227793077304459,
-0.200453310582776,-0.154190090601721,-0.0736931236097356,-0.0424502065788514,
0.),.UNSPECIFIED.);
#468=B_SPLINE_CURVE_WITH_KNOTS('',3,(#17982,#17983,#17984,#17985,#17986,
#17987,#17988,#17989,#17990,#17991),.UNSPECIFIED.,.F.,.F.,(4,2,2,2,4),(-0.479798392316289,
-0.37630045469605,-0.276804242240997,-0.133663587531333,0.),
 .UNSPECIFIED.);
#469=B_SPLINE_CURVE_WITH_KNOTS('',3,(#17996,#17997,#17998,#17999,#18000,
#18001,#18002,#18003,#18004,#18005,#18006,#18007,#18008,#18009),
 .UNSPECIFIED.,.F.,.F.,(4,2,2,2,2,2,4),(-0.255031134442356,-0.227793077291177,
-0.200453310572288,-0.154190090596086,-0.0736931236086164,-0.0424502065785607,
0.),.UNSPECIFIED.);
#470=B_SPLINE_CURVE_WITH_KNOTS('',3,(#18011,#18012,#18013,#18014,#18015,
#18016,#18017,#18018,#18019,#18020),.UNSPECIFIED.,.F.,.F.,(4,2,2,2,4),(-0.479798392585983,
-0.37630045488836,-0.276804242358604,-0.133663587557499,0.),
 .UNSPECIFIED.);
#471=B_SPLINE_CURVE_WITH_KNOTS('',3,(#18025,#18026,#18027,#18028,#18029,
#18030,#18031,#18032,#18033,#18034,#18035,#18036,#18037,#18038),
 .UNSPECIFIED.,.F.,.F.,(4,2,2,2,2,2,4),(-0.255031134477192,-0.227793077319635,
-0.200453310596239,-0.154190090616096,-0.0736931236157987,-0.0424502065810278,
0.),.UNSPECIFIED.);
#472=B_SPLINE_CURVE_WITH_KNOTS('',3,(#18040,#18041,#18042,#18043,#18044,
#18045,#18046,#18047,#18048,#18049),.UNSPECIFIED.,.F.,.F.,(4,2,2,2,4),(-0.479798392969913,
-0.376300455164432,-0.276804242530612,-0.133663587597497,0.),
 .UNSPECIFIED.);
#473=B_SPLINE_CURVE_WITH_KNOTS('',3,(#18054,#18055,#18056,#18057,#18058,
#18059,#18060,#18061,#18062,#18063,#18064,#18065,#18066,#18067),
 .UNSPECIFIED.,.F.,.F.,(4,2,2,2,2,2,4),(-0.255031134454417,-0.227793077300734,
-0.200453310579618,-0.154190090600756,-0.0736931236102396,-0.0424502065790721,
0.),.UNSPECIFIED.);
#474=B_SPLINE_CURVE_WITH_KNOTS('',3,(#18069,#18070,#18071,#18072,#18073,
#18074,#18075,#18076,#18077,#18078),.UNSPECIFIED.,.F.,.F.,(4,2,2,2,4),(-0.479798391685298,
-0.376300454251086,-0.276804241974231,-0.13366358747526,0.),
 .UNSPECIFIED.);
#475=B_SPLINE_CURVE_WITH_KNOTS('',3,(#18093,#18094,#18095,#18096,#18097,
#18098,#18099,#18100,#18101,#18102,#18103,#18104,#18105,#18106),
 .UNSPECIFIED.,.F.,.F.,(4,2,2,2,2,2,4),(-0.255031134441405,-0.227793077289669,
-0.200453310571579,-0.154190090599269,-0.073693123610816,-0.0424502065793788,
0.),.UNSPECIFIED.);
#476=B_SPLINE_CURVE_WITH_KNOTS('',3,(#18108,#18109,#18110,#18111,#18112,
#18113,#18114,#18115,#18116,#18117),.UNSPECIFIED.,.F.,.F.,(4,2,2,2,4),(-0.47979839202925,
-0.37630045448809,-0.276804242109191,-0.13366358749908,0.),
 .UNSPECIFIED.);
#477=B_SPLINE_CURVE_WITH_KNOTS('',3,(#18145,#18146,#18147,#18148,#18149,
#18150,#18151,#18152,#18153,#18154,#18155,#18156,#18157,#18158,#18159,#18160,
#18161,#18162,#18163,#18164,#18165,#18166,#18167,#18168,#18169,#18170,#18171,
#18172),.UNSPECIFIED.,.F.,.F.,(4,3,3,3,3,3,3,3,3,4),(0.,0.10419502125344,
0.208837694316349,0.315309080210678,0.394143302470623,0.474642117912927,
0.555269967633744,0.636143661419361,0.718213150424091,0.797153516796196),
 .UNSPECIFIED.);
#478=B_SPLINE_CURVE_WITH_KNOTS('',3,(#18205,#18206,#18207,#18208,#18209,
#18210,#18211,#18212,#18213,#18214,#18215,#18216,#18217,#18218,#18219,#18220,
#18221,#18222,#18223,#18224,#18225,#18226,#18227,#18228,#18229,#18230,#18231,
#18232),.UNSPECIFIED.,.F.,.F.,(4,3,3,3,3,3,3,3,3,4),(0.,0.104195149650902,
0.208837865524772,0.315309089419264,0.394143302470425,0.474642042092398,
0.555269910768279,0.636143270035123,0.718211827223173,0.797153516795923),
 .UNSPECIFIED.);
#479=B_SPLINE_CURVE_WITH_KNOTS('',3,(#18265,#18266,#18267,#18268,#18269,
#18270,#18271,#18272,#18273,#18274,#18275,#18276,#18277,#18278,#18279,#18280,
#18281,#18282,#18283,#18284,#18285,#18286,#18287,#18288,#18289,#18290,#18291,
#18292),.UNSPECIFIED.,.F.,.F.,(4,3,3,3,3,3,3,3,3,4),(0.,0.104195119607756,
0.208837825459222,0.315309087260799,0.394143302470401,0.474642059835697,
0.555269924075725,0.636143361633792,0.718212136889593,0.797153516795811),
 .UNSPECIFIED.);
#480=B_SPLINE_CURVE_WITH_KNOTS('',3,(#18325,#18326,#18327,#18328,#18329,
#18330,#18331,#18332,#18333,#18334,#18335,#18336,#18337,#18338,#18339,#18340,
#18341,#18342,#18343,#18344,#18345,#18346,#18347,#18348,#18349,#18350,#18351,
#18352),.UNSPECIFIED.,.F.,.F.,(4,3,3,3,3,3,3,3,3,4),(0.,0.104194925859371,
0.208837567155458,0.315309073394225,0.394143302470344,0.474642174225039,
0.555270009867713,0.636143952047701,0.718214133082137,0.797153516795737),
 .UNSPECIFIED.);
#481=B_SPLINE_CURVE_WITH_KNOTS('',3,(#18385,#18386,#18387,#18388,#18389,
#18390,#18391,#18392,#18393,#18394,#18395,#18396,#18397,#18398,#18399,#18400,
#18401,#18402,#18403,#18404,#18405,#18406,#18407,#18408,#18409,#18410,#18411,
#18412),.UNSPECIFIED.,.F.,.F.,(4,3,3,3,3,3,3,3,3,4),(0.,0.104194711471012,
0.208837281501618,0.315309058162189,0.394143302470344,0.47464230072316,
0.555270104741296,0.636144604731537,0.71821634019969,0.797153516795704),
 .UNSPECIFIED.);
#482=B_SPLINE_CURVE_WITH_KNOTS('',3,(#18445,#18446,#18447,#18448,#18449,
#18450,#18451,#18452,#18453,#18454,#18455,#18456,#18457,#18458,#18459,#18460,
#18461,#18462,#18463,#18464,#18465,#18466,#18467,#18468,#18469,#18470,#18471,
#18472),.UNSPECIFIED.,.F.,.F.,(4,3,3,3,3,3,3,3,3,4),(0.,0.104195021253205,
0.208837694315724,0.315309080210004,0.394143302470563,0.474642117912995,
0.555269967633764,0.636143661419282,0.718213150423912,0.797153516796073),
 .UNSPECIFIED.);
#483=B_SPLINE_CURVE_WITH_KNOTS('',3,(#18505,#18506,#18507,#18508,#18509,
#18510,#18511,#18512,#18513,#18514,#18515,#18516,#18517,#18518,#18519,#18520,
#18521,#18522,#18523,#18524,#18525,#18526,#18527,#18528,#18529,#18530,#18531,
#18532),.UNSPECIFIED.,.F.,.F.,(4,3,3,3,3,3,3,3,3,4),(0.,0.104195149651105,
0.208837865524873,0.315309089419088,0.394143302470483,0.474642042092258,
0.555269910768202,0.636143270034896,0.718211827223,0.797153516796034),
 .UNSPECIFIED.);
#484=B_SPLINE_CURVE_WITH_KNOTS('',3,(#18565,#18566,#18567,#18568,#18569,
#18570,#18571,#18572,#18573,#18574,#18575,#18576,#18577,#18578,#18579,#18580,
#18581,#18582,#18583,#18584,#18585,#18586,#18587,#18588,#18589,#18590,#18591,
#18592),.UNSPECIFIED.,.F.,.F.,(4,3,3,3,3,3,3,3,3,4),(0.,0.104195119607856,
0.208837825459762,0.315309087261884,0.394143302470623,0.474642059835987,
0.555269924076029,0.636143361634067,0.718212136889809,0.797153516796157),
 .UNSPECIFIED.);
#485=B_SPLINE_CURVE_WITH_KNOTS('',3,(#18625,#18626,#18627,#18628,#18629,
#18630,#18631,#18632,#18633,#18634,#18635,#18636,#18637,#18638,#18639,#18640,
#18641,#18642,#18643,#18644,#18645,#18646,#18647,#18648,#18649,#18650,#18651,
#18652),.UNSPECIFIED.,.F.,.F.,(4,3,3,3,3,3,3,3,3,4),(0.,0.104194925859672,
0.208837567155869,0.31530907339494,0.394143302470401,0.474642174225063,
0.555270009867749,0.636143952047726,0.71821413308218,0.797153516795805),
 .UNSPECIFIED.);
#486=B_SPLINE_CURVE_WITH_KNOTS('',3,(#18685,#18686,#18687,#18688,#18689,
#18690,#18691,#18692,#18693,#18694,#18695,#18696,#18697,#18698,#18699,#18700,
#18701,#18702,#18703,#18704,#18705,#18706,#18707,#18708,#18709,#18710,#18711,
#18712),.UNSPECIFIED.,.F.,.F.,(4,3,3,3,3,3,3,3,3,4),(0.,0.104194711471136,
0.208837281501506,0.315309058162058,0.394143302470353,0.474642300722815,
0.555270104741049,0.636144604731284,0.718216340199488,0.797153516795751),
 .UNSPECIFIED.);
#487=B_SPLINE_CURVE_WITH_KNOTS('',3,(#18745,#18746,#18747,#18748,#18749,
#18750,#18751,#18752,#18753,#18754,#18755,#18756,#18757,#18758,#18759,#18760,
#18761,#18762,#18763,#18764,#18765,#18766,#18767,#18768,#18769,#18770,#18771,
#18772),.UNSPECIFIED.,.F.,.F.,(4,3,3,3,3,3,3,3,3,4),(0.,0.104195021253541,
0.208837694316027,0.315309080210591,0.394143302470527,0.474642117912781,
0.555269967633599,0.636143661419217,0.718213150423855,0.797153516796053),
 .UNSPECIFIED.);
#488=B_SPLINE_CURVE_WITH_KNOTS('',3,(#18805,#18806,#18807,#18808,#18809,
#18810,#18811,#18812,#18813,#18814,#18815,#18816,#18817,#18818,#18819,#18820,
#18821,#18822,#18823,#18824,#18825,#18826,#18827,#18828,#18829,#18830,#18831,
#18832),.UNSPECIFIED.,.F.,.F.,(4,3,3,3,3,3,3,3,3,4),(0.,0.104195149650553,
0.208837865524795,0.315309089419618,0.394143302470498,0.474642042092278,
0.555269910768226,0.636143270034951,0.718211827223001,0.797153516796067),
 .UNSPECIFIED.);
#489=B_SPLINE_CURVE_WITH_KNOTS('',3,(#18865,#18866,#18867,#18868,#18869,
#18870,#18871,#18872,#18873,#18874,#18875,#18876,#18877,#18878,#18879,#18880,
#18881,#18882,#18883,#18884,#18885,#18886,#18887,#18888,#18889,#18890,#18891,
#18892),.UNSPECIFIED.,.F.,.F.,(4,3,3,3,3,3,3,3,3,4),(0.,0.104195119607818,
0.208837825459189,0.315309087261459,0.394143302470449,0.474642059835694,
0.555269924075731,0.636143361633688,0.718212136889352,0.797153516795842),
 .UNSPECIFIED.);
#490=B_SPLINE_CURVE_WITH_KNOTS('',3,(#18925,#18926,#18927,#18928,#18929,
#18930,#18931,#18932,#18933,#18934,#18935,#18936,#18937,#18938,#18939,#18940,
#18941,#18942,#18943,#18944,#18945,#18946,#18947,#18948,#18949,#18950,#18951,
#18952),.UNSPECIFIED.,.F.,.F.,(4,3,3,3,3,3,3,3,3,4),(0.,0.104194925859784,
0.208837567155939,0.31530907339513,0.394143302470471,0.474642174225348,
0.555270009867996,0.636143952047895,0.718214133082319,0.797153516795942),
 .UNSPECIFIED.);
#491=B_SPLINE_CURVE_WITH_KNOTS('',3,(#18985,#18986,#18987,#18988,#18989,
#18990,#18991,#18992,#18993,#18994,#18995,#18996,#18997,#18998,#18999,#19000,
#19001,#19002,#19003,#19004,#19005,#19006,#19007,#19008,#19009,#19010,#19011,
#19012),.UNSPECIFIED.,.F.,.F.,(4,3,3,3,3,3,3,3,3,4),(0.,0.104194711471186,
0.208837281501366,0.315309058162388,0.394143302470451,0.474642300723038,
0.555270104741255,0.636144604731555,0.718216340199711,0.797153516795907),
 .UNSPECIFIED.);
#492=B_SPLINE_CURVE_WITH_KNOTS('',3,(#19045,#19046,#19047,#19048,#19049,
#19050,#19051,#19052,#19053,#19054,#19055,#19056,#19057,#19058,#19059,#19060,
#19061,#19062,#19063,#19064,#19065,#19066,#19067,#19068,#19069,#19070,#19071,
#19072),.UNSPECIFIED.,.F.,.F.,(4,3,3,3,3,3,3,3,3,4),(0.,0.104195021253042,
0.208837694315628,0.315309080210067,0.394143302470476,0.474642117912826,
0.55526996763361,0.636143661419199,0.718213150423859,0.797153516795962),
 .UNSPECIFIED.);
#493=B_SPLINE_CURVE_WITH_KNOTS('',3,(#19105,#19106,#19107,#19108,#19109,
#19110,#19111,#19112,#19113,#19114,#19115,#19116,#19117,#19118,#19119,#19120,
#19121,#19122,#19123,#19124,#19125,#19126,#19127,#19128,#19129,#19130,#19131,
#19132),.UNSPECIFIED.,.F.,.F.,(4,3,3,3,3,3,3,3,3,4),(0.,0.104195149650775,
0.208837865524784,0.315309089419042,0.394143302470323,0.474642042092065,
0.555269910767973,0.636143270034795,0.71821182722283,0.797153516795697),
 .UNSPECIFIED.);
#494=B_SPLINE_CURVE_WITH_KNOTS('',3,(#19165,#19166,#19167,#19168,#19169,
#19170,#19171,#19172,#19173,#19174,#19175,#19176,#19177,#19178,#19179,#19180,
#19181,#19182,#19183,#19184,#19185,#19186,#19187,#19188,#19189,#19190,#19191,
#19192),.UNSPECIFIED.,.F.,.F.,(4,3,3,3,3,3,3,3,3,4),(0.,0.104195119607863,
0.208837825459412,0.31530908726121,0.394143302470542,0.474642059835598,
0.555269924075699,0.63614336163368,0.718212136889433,0.797153516796002),
 .UNSPECIFIED.);
#495=B_SPLINE_CURVE_WITH_KNOTS('',3,(#19225,#19226,#19227,#19228,#19229,
#19230,#19231,#19232,#19233,#19234,#19235,#19236,#19237,#19238,#19239,#19240,
#19241,#19242,#19243,#19244,#19245,#19246,#19247,#19248,#19249,#19250,#19251,
#19252),.UNSPECIFIED.,.F.,.F.,(4,3,3,3,3,3,3,3,3,4),(0.,0.104194925859466,
0.208837567155331,0.315309073394099,0.394143302470382,0.474642174224968,
0.555270009867677,0.636143952047661,0.718214133082044,0.797153516795802),
 .UNSPECIFIED.);
#496=B_SPLINE_CURVE_WITH_KNOTS('',3,(#19285,#19286,#19287,#19288,#19289,
#19290,#19291,#19292,#19293,#19294,#19295,#19296,#19297,#19298,#19299,#19300,
#19301,#19302,#19303,#19304,#19305,#19306,#19307,#19308,#19309,#19310,#19311,
#19312),.UNSPECIFIED.,.F.,.F.,(4,3,3,3,3,3,3,3,3,4),(0.,0.104194711470983,
0.208837281501467,0.315309058162056,0.394143302470363,0.474642300723069,
0.555270104741244,0.636144604731482,0.718216340199667,0.797153516795768),
 .UNSPECIFIED.);
#497=B_SPLINE_CURVE_WITH_KNOTS('',3,(#19370,#19371,#19372,#19373,#19374,
#19375,#19376,#19377,#19378,#19379,#19380,#19381,#19382,#19383,#19384,#19385,
#19386,#19387,#19388,#19389,#19390,#19391,#19392,#19393,#19394,#19395,#19396,
#19397),.UNSPECIFIED.,.F.,.F.,(4,3,3,3,3,3,3,3,3,4),(0.,0.0913693045581491,
0.175304752632241,0.256829545365516,0.336180776983803,0.39678509935003,
0.504865678023162,0.611029081983863,0.715415587626191,0.795801737615653),
 .UNSPECIFIED.);
#498=B_SPLINE_CURVE_WITH_KNOTS('',3,(#19405,#19406,#19407,#19408,#19409,
#19410,#19411,#19412,#19413,#19414,#19415,#19416,#19417,#19418,#19419,#19420,
#19421,#19422,#19423,#19424,#19425,#19426,#19427,#19428,#19429,#19430,#19431,
#19432),.UNSPECIFIED.,.F.,.F.,(4,3,3,3,3,3,3,3,3,4),(0.,0.091300847639123,
0.17522519587234,0.256743850114013,0.336091868063455,0.396785099350019,
0.50484847748811,0.610985103772719,0.715329935719015,0.795801737615632),
 .UNSPECIFIED.);
#499=B_SPLINE_CURVE_WITH_KNOTS('',3,(#19435,#19436,#19437,#19438,#19439,
#19440,#19441,#19442,#19443,#19444,#19445,#19446,#19447,#19448,#19449,#19450,
#19451,#19452,#19453,#19454,#19455,#19456,#19457,#19458,#19459,#19460,#19461,
#19462),.UNSPECIFIED.,.F.,.F.,(4,3,3,3,3,3,3,3,3,4),(0.,0.0913055244675908,
0.175231740459174,0.256751333955076,0.336099680903453,0.396785099350007,
0.504849076375648,0.610985832253314,0.715329675493193,0.795801737615589),
 .UNSPECIFIED.);
#500=B_SPLINE_CURVE_WITH_KNOTS('',3,(#19465,#19466,#19467,#19468,#19469,
#19470,#19471,#19472,#19473,#19474,#19475,#19476,#19477,#19478,#19479,#19480,
#19481,#19482,#19483,#19484,#19485,#19486,#19487,#19488,#19489,#19490,#19491,
#19492),.UNSPECIFIED.,.F.,.F.,(4,3,3,3,3,3,3,3,3,4),(0.,0.0913671480398549,
0.1753017609357,0.256826133349693,0.336177213290906,0.396785099349999,0.504865390200783,
0.611028723085786,0.71541568566786,0.795801737615528),.UNSPECIFIED.);
#501=B_SPLINE_CURVE_WITH_KNOTS('',3,(#19495,#19496,#19497,#19498,#19499,
#19500,#19501,#19502,#19503,#19504,#19505,#19506,#19507,#19508,#19509,#19510,
#19511,#19512,#19513,#19514,#19515,#19516,#19517,#19518,#19519,#19520,#19521,
#19522),.UNSPECIFIED.,.F.,.F.,(4,3,3,3,3,3,3,3,3,4),(0.,0.0913693045581935,
0.175304752632336,0.256829545365578,0.336180776983921,0.396785099350045,
0.504865678023515,0.611029081984597,0.715415587626544,0.795801737615703),
 .UNSPECIFIED.);
#502=B_SPLINE_CURVE_WITH_KNOTS('',3,(#19525,#19526,#19527,#19528,#19529,
#19530,#19531,#19532,#19533,#19534,#19535,#19536,#19537,#19538,#19539,#19540,
#19541,#19542,#19543,#19544,#19545,#19546,#19547,#19548,#19549,#19550,#19551,
#19552),.UNSPECIFIED.,.F.,.F.,(4,3,3,3,3,3,3,3,3,4),(0.,0.0913663024514722,
0.175300588104174,0.256824795817819,0.336175816276576,0.396785099350014,
0.504865277207551,0.611028582106192,0.71541572388289,0.795801737615583),
 .UNSPECIFIED.);
#503=B_SPLINE_CURVE_WITH_KNOTS('',3,(#19555,#19556,#19557,#19558,#19559,
#19560,#19561,#19562,#19563,#19564,#19565,#19566,#19567,#19568,#19569,#19570,
#19571,#19572,#19573,#19574,#19575,#19576,#19577,#19578,#19579,#19580,#19581,
#19582),.UNSPECIFIED.,.F.,.F.,(4,3,3,3,3,3,3,3,3,4),(0.,0.0913008476389673,
0.175225195872217,0.256743850113661,0.3360918680631,0.396785099350015,0.504848477488003,
0.610985103772403,0.715329935719092,0.795801737615593),.UNSPECIFIED.);
#504=B_SPLINE_CURVE_WITH_KNOTS('',3,(#19585,#19586,#19587,#19588,#19589,
#19590,#19591,#19592,#19593,#19594,#19595,#19596,#19597,#19598,#19599,#19600,
#19601,#19602,#19603,#19604,#19605,#19606,#19607,#19608,#19609,#19610,#19611,
#19612),.UNSPECIFIED.,.F.,.F.,(4,3,3,3,3,3,3,3,3,4),(0.,0.0913055244674033,
0.175231740458983,0.256751333954684,0.336099680903084,0.396785099350008,
0.504849076375157,0.610985832252606,0.715329675492173,0.795801737615577),
 .UNSPECIFIED.);
#505=B_SPLINE_CURVE_WITH_KNOTS('',3,(#19615,#19616,#19617,#19618,#19619,
#19620,#19621,#19622,#19623,#19624,#19625,#19626,#19627,#19628,#19629,#19630,
#19631,#19632,#19633,#19634,#19635,#19636,#19637,#19638,#19639,#19640,#19641,
#19642),.UNSPECIFIED.,.F.,.F.,(4,3,3,3,3,3,3,3,3,4),(0.,0.0913671480397717,
0.175301760935616,0.256826133349839,0.33617721329114,0.396785099349993,
0.504865390200107,0.611028723084967,0.715415685666501,0.795801737615502),
 .UNSPECIFIED.);
#506=B_SPLINE_CURVE_WITH_KNOTS('',3,(#19645,#19646,#19647,#19648,#19649,
#19650,#19651,#19652,#19653,#19654,#19655,#19656,#19657,#19658,#19659,#19660,
#19661,#19662,#19663,#19664,#19665,#19666,#19667,#19668,#19669,#19670,#19671,
#19672),.UNSPECIFIED.,.F.,.F.,(4,3,3,3,3,3,3,3,3,4),(0.,0.0913663024513228,
0.175300588104033,0.256824795817617,0.336175816276443,0.396785099350013,
0.504865277207549,0.61102858210682,0.715415723883384,0.795801737615587),
 .UNSPECIFIED.);
#507=B_SPLINE_CURVE_WITH_KNOTS('',3,(#19675,#19676,#19677,#19678,#19679,
#19680,#19681,#19682,#19683,#19684,#19685,#19686,#19687,#19688,#19689,#19690,
#19691,#19692,#19693,#19694,#19695,#19696,#19697,#19698,#19699,#19700,#19701,
#19702),.UNSPECIFIED.,.F.,.F.,(4,3,3,3,3,3,3,3,3,4),(0.,0.0913008476389372,
0.175225195872126,0.256743850113633,0.336091868062983,0.396785099350007,
0.504848477488055,0.610985103772565,0.715329935719059,0.795801737615582),
 .UNSPECIFIED.);
#508=B_SPLINE_CURVE_WITH_KNOTS('',3,(#19705,#19706,#19707,#19708,#19709,
#19710,#19711,#19712,#19713,#19714,#19715,#19716,#19717,#19718,#19719,#19720,
#19721,#19722,#19723,#19724,#19725,#19726,#19727,#19728,#19729,#19730,#19731,
#19732),.UNSPECIFIED.,.F.,.F.,(4,3,3,3,3,3,3,3,3,4),(0.,0.0913055244673888,
0.175231740458997,0.256751333954802,0.336099680903054,0.396785099350015,
0.504849076375127,0.610985832252708,0.715329675492648,0.795801737615576),
 .UNSPECIFIED.);
#509=B_SPLINE_CURVE_WITH_KNOTS('',3,(#19735,#19736,#19737,#19738,#19739,
#19740,#19741,#19742,#19743,#19744,#19745,#19746,#19747,#19748,#19749,#19750,
#19751,#19752,#19753,#19754,#19755,#19756,#19757,#19758,#19759,#19760,#19761,
#19762),.UNSPECIFIED.,.F.,.F.,(4,3,3,3,3,3,3,3,3,4),(0.,0.0913671480401054,
0.175301760935917,0.256826133350214,0.336177213291394,0.396785099349986,
0.504865390200262,0.611028723085204,0.715415685667019,0.795801737615469),
 .UNSPECIFIED.);
#510=B_SPLINE_CURVE_WITH_KNOTS('',3,(#19765,#19766,#19767,#19768,#19769,
#19770,#19771,#19772,#19773,#19774,#19775,#19776,#19777,#19778,#19779,#19780,
#19781,#19782,#19783,#19784,#19785,#19786,#19787,#19788,#19789,#19790,#19791,
#19792),.UNSPECIFIED.,.F.,.F.,(4,3,3,3,3,3,3,3,3,4),(0.,0.0913693045578756,
0.175304752632037,0.256829545365211,0.336180776983551,0.396785099350051,
0.504865678023637,0.611029081985028,0.715415587627274,0.79580173761574),
 .UNSPECIFIED.);
#511=B_SPLINE_CURVE_WITH_KNOTS('',3,(#19795,#19796,#19797,#19798,#19799,
#19800,#19801,#19802,#19803,#19804,#19805,#19806,#19807,#19808,#19809,#19810,
#19811,#19812,#19813,#19814,#19815,#19816,#19817,#19818,#19819,#19820,#19821,
#19822),.UNSPECIFIED.,.F.,.F.,(4,3,3,3,3,3,3,3,3,4),(0.,0.0913663024515618,
0.175300588104283,0.256824795817736,0.336175816276531,0.396785099350011,
0.504865277207547,0.611028582106704,0.715415723883272,0.795801737615553),
 .UNSPECIFIED.);
#512=B_SPLINE_CURVE_WITH_KNOTS('',3,(#19825,#19826,#19827,#19828,#19829,
#19830,#19831,#19832,#19833,#19834,#19835,#19836,#19837,#19838,#19839,#19840,
#19841,#19842,#19843,#19844,#19845,#19846,#19847,#19848,#19849,#19850,#19851,
#19852),.UNSPECIFIED.,.F.,.F.,(4,3,3,3,3,3,3,3,3,4),(0.,0.0913008476390098,
0.175225195872273,0.256743850113871,0.3360918680633,0.396785099350018,0.5048484774884,
0.610985103772909,0.715329935719289,0.795801737615643),.UNSPECIFIED.);
#513=B_SPLINE_CURVE_WITH_KNOTS('',3,(#19855,#19856,#19857,#19858,#19859,
#19860,#19861,#19862,#19863,#19864,#19865,#19866,#19867,#19868,#19869,#19870,
#19871,#19872,#19873,#19874,#19875,#19876,#19877,#19878,#19879,#19880,#19881,
#19882),.UNSPECIFIED.,.F.,.F.,(4,3,3,3,3,3,3,3,3,4),(0.,0.0913055244672643,
0.175231740458797,0.256751333954625,0.336099680903062,0.396785099349991,
0.504849076374745,0.610985832251881,0.715329675491931,0.795801737615494),
 .UNSPECIFIED.);
#514=B_SPLINE_CURVE_WITH_KNOTS('',3,(#19885,#19886,#19887,#19888,#19889,
#19890,#19891,#19892,#19893,#19894,#19895,#19896,#19897,#19898,#19899,#19900,
#19901,#19902,#19903,#19904,#19905,#19906,#19907,#19908,#19909,#19910,#19911,
#19912),.UNSPECIFIED.,.F.,.F.,(4,3,3,3,3,3,3,3,3,4),(0.,0.0913671480398292,
0.175301760935665,0.256826133349879,0.336177213291251,0.396785099350001,
0.504865390199928,0.611028723084993,0.715415685666863,0.795801737615546),
 .UNSPECIFIED.);
#515=B_SPLINE_CURVE_WITH_KNOTS('',3,(#19915,#19916,#19917,#19918,#19919,
#19920,#19921,#19922,#19923,#19924,#19925,#19926,#19927,#19928,#19929,#19930,
#19931,#19932,#19933,#19934,#19935,#19936,#19937,#19938,#19939,#19940,#19941,
#19942),.UNSPECIFIED.,.F.,.F.,(4,3,3,3,3,3,3,3,3,4),(0.,0.0913693045582462,
0.175304752632388,0.256829545365668,0.336180776983957,0.396785099350025,
0.50486567802321,0.6110290819841,0.715415587626411,0.795801737615617),
 .UNSPECIFIED.);
#516=B_SPLINE_CURVE_WITH_KNOTS('',3,(#19945,#19946,#19947,#19948,#19949,
#19950,#19951,#19952,#19953,#19954,#19955,#19956,#19957,#19958,#19959,#19960,
#19961,#19962,#19963,#19964,#19965,#19966,#19967,#19968,#19969,#19970,#19971,
#19972),.UNSPECIFIED.,.F.,.F.,(4,3,3,3,3,3,3,3,3,4),(0.,0.0913663024513698,
0.175300588104129,0.256824795817702,0.336175816276519,0.396785099350012,
0.504865277207553,0.611028582106785,0.71541572388335,0.795801737615573),
 .UNSPECIFIED.);
#517=B_SPLINE_CURVE_WITH_KNOTS('',3,(#21115,#21116,#21117,#21118,#21119,
#21120),.UNSPECIFIED.,.F.,.F.,(4,2,4),(0.226218361876484,0.25919316472602,
0.292167967575556),.UNSPECIFIED.);
#518=B_SPLINE_CURVE_WITH_KNOTS('',3,(#21122,#21123,#21124,#21125,#21126,
#21127,#21128,#21129,#21130,#21131,#21132),.UNSPECIFIED.,.F.,.F.,(4,2,3,
2,4),(-0.170336741191592,-0.0873737681171707,0.,0.0873737681171706,0.170336741191592),
 .UNSPECIFIED.);
#519=B_SPLINE_CURVE_WITH_KNOTS('',3,(#21134,#21135,#21136,#21137,#21138,
#21139),.UNSPECIFIED.,.F.,.F.,(4,2,4),(0.958318332016868,0.991720601129839,
1.02512287024281),.UNSPECIFIED.);
#520=B_SPLINE_CURVE_WITH_KNOTS('',3,(#21140,#21141,#21142,#21143,#21144,
#21145,#21146,#21147,#21148,#21149,#21150),.UNSPECIFIED.,.F.,.F.,(4,2,3,
2,4),(-0.170336741191593,-0.0873737681171707,0.,0.0873737681171707,0.170336741191592),
 .UNSPECIFIED.);
#521=B_SPLINE_CURVE_WITH_KNOTS('',3,(#21153,#21154,#21155,#21156,#21157,
#21158),.UNSPECIFIED.,.F.,.F.,(4,2,4),(0.699168310489759,0.727019400778947,
0.754870491068134),.UNSPECIFIED.);
#522=B_SPLINE_CURVE_WITH_KNOTS('',3,(#21160,#21161,#21162,#21163,#21164,
#21165,#21166,#21167,#21168,#21169),.UNSPECIFIED.,.F.,.F.,(4,2,2,2,4),(0.528720639901106,
0.611686436801216,0.699059005116263,0.78643157343131,0.869397370331421),
 .UNSPECIFIED.);
#523=B_SPLINE_CURVE_WITH_KNOTS('',3,(#21171,#21172,#21173,#21174,#21175,
#21176),.UNSPECIFIED.,.F.,.F.,(4,2,4),(0.21448870997046,0.242339800259649,
0.270190890548838),.UNSPECIFIED.);
#524=B_SPLINE_CURVE_WITH_KNOTS('',3,(#21177,#21178,#21179,#21180,#21181,
#21182,#21183,#21184,#21185,#21186),.UNSPECIFIED.,.F.,.F.,(4,2,2,2,4),(0.528720639901106,
0.611686436801217,0.699059005116263,0.78643157343131,0.869397370331421),
 .UNSPECIFIED.);
#525=B_SPLINE_CURVE_WITH_KNOTS('',3,(#21193,#21194,#21195,#21196),
 .UNSPECIFIED.,.F.,.F.,(4,4),(0.991720601129836,1.02512287024281),
 .UNSPECIFIED.);
#526=B_SPLINE_CURVE_WITH_KNOTS('',3,(#21200,#21201,#21202,#21203,#21204,
#21205),.UNSPECIFIED.,.F.,.F.,(4,2,4),(0.958318332016865,0.991720601129836,
1.02512287024281),.UNSPECIFIED.);
#527=B_SPLINE_CURVE_WITH_KNOTS('',3,(#21209,#21210,#21211,#21212,#21213,
#21214),.UNSPECIFIED.,.F.,.F.,(4,2,4),(0.958318332016865,0.991720601129836,
1.02512287024281),.UNSPECIFIED.);
#528=B_SPLINE_CURVE_WITH_KNOTS('',3,(#21218,#21219,#21220,#21221,#21222,
#21223),.UNSPECIFIED.,.F.,.F.,(4,2,4),(0.958318332016865,0.991720601129836,
1.02512287024281),.UNSPECIFIED.);
#529=B_SPLINE_CURVE_WITH_KNOTS('',3,(#21227,#21228,#21229,#21230,#21231,
#21232),.UNSPECIFIED.,.F.,.F.,(4,2,4),(0.958318332016865,0.991720601129836,
1.02512287024281),.UNSPECIFIED.);
#530=B_SPLINE_CURVE_WITH_KNOTS('',3,(#21236,#21237,#21238,#21239,#21240,
#21241),.UNSPECIFIED.,.F.,.F.,(4,2,4),(0.958318332016865,0.991720601129836,
1.02512287024281),.UNSPECIFIED.);
#531=B_SPLINE_CURVE_WITH_KNOTS('',3,(#21246,#21247,#21248,#21249,#21250,
#21251),.UNSPECIFIED.,.F.,.F.,(4,2,4),(0.958318332016865,0.991720601129837,
1.02512287024281),.UNSPECIFIED.);
#532=B_SPLINE_CURVE_WITH_KNOTS('',3,(#21255,#21256,#21257,#21258,#21259,
#21260),.UNSPECIFIED.,.F.,.F.,(4,2,4),(0.958318332016865,0.991720601129836,
1.02512287024281),.UNSPECIFIED.);
#533=B_SPLINE_CURVE_WITH_KNOTS('',3,(#21264,#21265,#21266,#21267,#21268,
#21269),.UNSPECIFIED.,.F.,.F.,(4,2,4),(0.958318332016866,0.99172060112984,
1.02512287024281),.UNSPECIFIED.);
#534=B_SPLINE_CURVE_WITH_KNOTS('',3,(#21272,#21273,#21274,#21275),
 .UNSPECIFIED.,.F.,.F.,(4,4),(0.958318332016865,0.991720601129836),
 .UNSPECIFIED.);
#535=B_SPLINE_CURVE_WITH_KNOTS('',3,(#21279,#21280,#21281,#21282,#21283,
#21284,#21285,#21286,#21287,#21288,#21289),.UNSPECIFIED.,.F.,.F.,(4,2,3,
2,4),(-0.170336741191593,-0.0873737681171707,0.,0.0873737681171707,0.170336741191592),
 .UNSPECIFIED.);
#536=B_SPLINE_CURVE_WITH_KNOTS('',3,(#21294,#21295,#21296,#21297,#21298,
#21299),.UNSPECIFIED.,.F.,.F.,(4,2,4),(0.21448870997046,0.242339800259649,
0.270190890548838),.UNSPECIFIED.);
#537=B_SPLINE_CURVE_WITH_KNOTS('',3,(#21303,#21304,#21305,#21306,#21307,
#21308),.UNSPECIFIED.,.F.,.F.,(4,2,4),(0.21448870997046,0.242339800259649,
0.270190890548838),.UNSPECIFIED.);
#538=B_SPLINE_CURVE_WITH_KNOTS('',3,(#21312,#21313,#21314,#21315,#21316,
#21317),.UNSPECIFIED.,.F.,.F.,(4,2,4),(0.21448870997046,0.242339800259649,
0.270190890548838),.UNSPECIFIED.);
#539=B_SPLINE_CURVE_WITH_KNOTS('',3,(#21321,#21322,#21323,#21324),
 .UNSPECIFIED.,.F.,.F.,(4,4),(0.21448870997046,0.242339800259649),
 .UNSPECIFIED.);
#540=B_SPLINE_CURVE_WITH_KNOTS('',3,(#21329,#21330,#21331,#21332),
 .UNSPECIFIED.,.F.,.F.,(4,4),(0.242339800259649,0.270190890548838),
 .UNSPECIFIED.);
#541=B_SPLINE_CURVE_WITH_KNOTS('',3,(#21336,#21337,#21338,#21339,#21340,
#21341),.UNSPECIFIED.,.F.,.F.,(4,2,4),(0.21448870997046,0.242339800259649,
0.270190890548838),.UNSPECIFIED.);
#542=B_SPLINE_CURVE_WITH_KNOTS('',3,(#21345,#21346,#21347,#21348,#21349,
#21350),.UNSPECIFIED.,.F.,.F.,(4,2,4),(0.21448870997046,0.242339800259649,
0.270190890548838),.UNSPECIFIED.);
#543=B_SPLINE_CURVE_WITH_KNOTS('',3,(#21354,#21355,#21356,#21357,#21358,
#21359),.UNSPECIFIED.,.F.,.F.,(4,2,4),(0.21448870997046,0.242339800259649,
0.270190890548838),.UNSPECIFIED.);
#544=B_SPLINE_CURVE_WITH_KNOTS('',3,(#21363,#21364,#21365,#21366,#21367,
#21368),.UNSPECIFIED.,.F.,.F.,(4,2,4),(0.21448870997046,0.242339800259649,
0.270190890548838),.UNSPECIFIED.);
#545=B_SPLINE_CURVE_WITH_KNOTS('',3,(#21372,#21373,#21374,#21375,#21376,
#21377),.UNSPECIFIED.,.F.,.F.,(4,2,4),(0.21448870997046,0.242339800259649,
0.270190890548838),.UNSPECIFIED.);
#546=B_SPLINE_CURVE_WITH_KNOTS('',3,(#21382,#21383,#21384,#21385,#21386,
#21387,#21388,#21389,#21390,#21391),.UNSPECIFIED.,.F.,.F.,(4,2,2,2,4),(0.528720639901106,
0.611686436801216,0.699059005116263,0.786431573431309,0.869397370331421),
 .UNSPECIFIED.);
#547=B_SPLINE_CURVE_WITH_KNOTS('',3,(#21397,#21398,#21399,#21400,#21401,
#21402),.UNSPECIFIED.,.F.,.F.,(4,2,4),(0.226218361876484,0.259193164726019,
0.292167967575555),.UNSPECIFIED.);
#548=B_SPLINE_CURVE_WITH_KNOTS('',3,(#21403,#21404,#21405,#21406,#21407,
#21408,#21409,#21410,#21411,#21412,#21413),.UNSPECIFIED.,.F.,.F.,(4,2,3,
2,4),(-0.170336741191593,-0.0873737681171707,0.,0.0873737681171706,0.170336741191593),
 .UNSPECIFIED.);
#549=B_SPLINE_CURVE_WITH_KNOTS('',3,(#21415,#21416,#21417,#21418,#21419,
#21420),.UNSPECIFIED.,.F.,.F.,(4,2,4),(0.69916831048976,0.727019400778947,
0.754870491068134),.UNSPECIFIED.);
#550=B_SPLINE_CURVE_WITH_KNOTS('',3,(#21421,#21422,#21423,#21424,#21425,
#21426,#21427,#21428,#21429,#21430),.UNSPECIFIED.,.F.,.F.,(4,2,2,2,4),(0.528720639901105,
0.611686436801216,0.699059005116263,0.786431573431309,0.86939737033142),
 .UNSPECIFIED.);
#551=B_SPLINE_CURVE_WITH_KNOTS('',3,(#21434,#21435,#21436,#21437,#21438,
#21439,#21440,#21441,#21442,#21443,#21444),.UNSPECIFIED.,.F.,.F.,(4,2,3,
2,4),(-0.170336741191592,-0.0873737681171707,0.,0.0873737681171709,0.170336741191593),
 .UNSPECIFIED.);
#552=B_SPLINE_CURVE_WITH_KNOTS('',3,(#21448,#21449,#21450,#21451,#21452,
#21453,#21454,#21455,#21456,#21457),.UNSPECIFIED.,.F.,.F.,(4,2,2,2,4),(0.528720639901106,
0.611686436801216,0.699059005116263,0.78643157343131,0.869397370331421),
 .UNSPECIFIED.);
#553=B_SPLINE_CURVE_WITH_KNOTS('',3,(#21463,#21464,#21465,#21466,#21467,
#21468),.UNSPECIFIED.,.F.,.F.,(4,2,4),(0.226218361876484,0.259193164726019,
0.292167967575555),.UNSPECIFIED.);
#554=B_SPLINE_CURVE_WITH_KNOTS('',3,(#21469,#21470,#21471,#21472,#21473,
#21474,#21475,#21476,#21477,#21478,#21479),.UNSPECIFIED.,.F.,.F.,(4,2,3,
2,4),(-0.170336741191593,-0.0873737681171709,0.,0.0873737681171706,0.170336741191592),
 .UNSPECIFIED.);
#555=B_SPLINE_CURVE_WITH_KNOTS('',3,(#21481,#21482,#21483,#21484,#21485,
#21486),.UNSPECIFIED.,.F.,.F.,(4,2,4),(0.69916831048976,0.727019400778947,
0.754870491068134),.UNSPECIFIED.);
#556=B_SPLINE_CURVE_WITH_KNOTS('',3,(#21487,#21488,#21489,#21490,#21491,
#21492,#21493,#21494,#21495,#21496),.UNSPECIFIED.,.F.,.F.,(4,2,2,2,4),(0.528720639901106,
0.611686436801216,0.699059005116263,0.78643157343131,0.869397370331421),
 .UNSPECIFIED.);
#557=B_SPLINE_CURVE_WITH_KNOTS('',3,(#21500,#21501,#21502,#21503,#21504,
#21505,#21506,#21507,#21508,#21509,#21510),.UNSPECIFIED.,.F.,.F.,(4,2,3,
2,4),(-0.170336741191593,-0.0873737681171707,0.,0.0873737681171706,0.170336741191593),
 .UNSPECIFIED.);
#558=B_SPLINE_CURVE_WITH_KNOTS('',3,(#21514,#21515,#21516,#21517,#21518,
#21519,#21520,#21521,#21522,#21523),.UNSPECIFIED.,.F.,.F.,(4,2,2,2,4),(0.528720639901106,
0.611686436801217,0.699059005116263,0.78643157343131,0.869397370331421),
 .UNSPECIFIED.);
#559=B_SPLINE_CURVE_WITH_KNOTS('',3,(#21529,#21530,#21531,#21532,#21533,
#21534),.UNSPECIFIED.,.F.,.F.,(4,2,4),(0.226218361876484,0.25919316472602,
0.292167967575555),.UNSPECIFIED.);
#560=B_SPLINE_CURVE_WITH_KNOTS('',3,(#21535,#21536,#21537,#21538,#21539,
#21540,#21541,#21542,#21543,#21544,#21545),.UNSPECIFIED.,.F.,.F.,(4,2,3,
2,4),(-0.170336741191592,-0.0873737681171705,0.,0.0873737681171705,0.170336741191593),
 .UNSPECIFIED.);
#561=B_SPLINE_CURVE_WITH_KNOTS('',3,(#21547,#21548,#21549,#21550,#21551,
#21552),.UNSPECIFIED.,.F.,.F.,(4,2,4),(0.699168310489759,0.727019400778946,
0.754870491068134),.UNSPECIFIED.);
#562=B_SPLINE_CURVE_WITH_KNOTS('',3,(#21553,#21554,#21555,#21556,#21557,
#21558,#21559,#21560,#21561,#21562),.UNSPECIFIED.,.F.,.F.,(4,2,2,2,4),(0.528720639901106,
0.611686436801216,0.699059005116263,0.786431573431309,0.86939737033142),
 .UNSPECIFIED.);
#563=B_SPLINE_CURVE_WITH_KNOTS('',3,(#21566,#21567,#21568,#21569,#21570,
#21571,#21572,#21573,#21574,#21575,#21576),.UNSPECIFIED.,.F.,.F.,(4,2,3,
2,4),(-0.170336741191593,-0.0873737681171707,0.,0.0873737681171707,0.170336741191592),
 .UNSPECIFIED.);
#564=B_SPLINE_CURVE_WITH_KNOTS('',3,(#21580,#21581,#21582,#21583,#21584,
#21585,#21586,#21587,#21588,#21589),.UNSPECIFIED.,.F.,.F.,(4,2,2,2,4),(0.528720639901106,
0.611686436801217,0.699059005116263,0.78643157343131,0.869397370331421),
 .UNSPECIFIED.);
#565=B_SPLINE_CURVE_WITH_KNOTS('',3,(#21596,#21597,#21598,#21599),
 .UNSPECIFIED.,.F.,.F.,(4,4),(0.226218361876484,0.259193164726019),
 .UNSPECIFIED.);
#566=B_SPLINE_CURVE_WITH_KNOTS('',3,(#21600,#21601,#21602,#21603,#21604,
#21605,#21606,#21607,#21608,#21609,#21610),.UNSPECIFIED.,.F.,.F.,(4,2,3,
2,4),(-0.170336741191593,-0.0873737681171707,0.,0.0873737681171706,0.170336741191593),
 .UNSPECIFIED.);
#567=B_SPLINE_CURVE_WITH_KNOTS('',3,(#21611,#21612,#21613,#21614),
 .UNSPECIFIED.,.F.,.F.,(4,4),(0.259193164726019,0.292167967575555),
 .UNSPECIFIED.);
#568=B_SPLINE_CURVE_WITH_KNOTS('',3,(#21617,#21618,#21619,#21620),
 .UNSPECIFIED.,.F.,.F.,(4,4),(0.69916831048976,0.727019400778947),
 .UNSPECIFIED.);
#569=B_SPLINE_CURVE_WITH_KNOTS('',3,(#21621,#21622,#21623,#21624,#21625,
#21626,#21627,#21628,#21629,#21630),.UNSPECIFIED.,.F.,.F.,(4,2,2,2,4),(0.528720639901106,
0.611686436801216,0.699059005116263,0.78643157343131,0.869397370331421),
 .UNSPECIFIED.);
#570=B_SPLINE_CURVE_WITH_KNOTS('',3,(#21631,#21632,#21633,#21634),
 .UNSPECIFIED.,.F.,.F.,(4,4),(0.727019400778947,0.754870491068135),
 .UNSPECIFIED.);
#571=B_SPLINE_CURVE_WITH_KNOTS('',3,(#21638,#21639,#21640,#21641,#21642,
#21643,#21644,#21645,#21646,#21647,#21648),.UNSPECIFIED.,.F.,.F.,(4,2,3,
2,4),(-0.170336741191592,-0.0873737681171705,0.,0.0873737681171706,0.170336741191592),
 .UNSPECIFIED.);
#572=B_SPLINE_CURVE_WITH_KNOTS('',3,(#21652,#21653,#21654,#21655,#21656,
#21657,#21658,#21659,#21660,#21661),.UNSPECIFIED.,.F.,.F.,(4,2,2,2,4),(0.528720639901106,
0.611686436801216,0.699059005116263,0.78643157343131,0.869397370331421),
 .UNSPECIFIED.);
#573=B_SPLINE_CURVE_WITH_KNOTS('',3,(#21667,#21668,#21669,#21670,#21671,
#21672),.UNSPECIFIED.,.F.,.F.,(4,2,4),(0.226218361876484,0.25919316472602,
0.292167967575555),.UNSPECIFIED.);
#574=B_SPLINE_CURVE_WITH_KNOTS('',3,(#21673,#21674,#21675,#21676,#21677,
#21678,#21679,#21680,#21681,#21682,#21683),.UNSPECIFIED.,.F.,.F.,(4,2,3,
2,4),(-0.170336741191592,-0.0873737681171707,0.,0.0873737681171706,0.170336741191592),
 .UNSPECIFIED.);
#575=B_SPLINE_CURVE_WITH_KNOTS('',3,(#21685,#21686,#21687,#21688,#21689,
#21690),.UNSPECIFIED.,.F.,.F.,(4,2,4),(0.69916831048976,0.727019400778947,
0.754870491068134),.UNSPECIFIED.);
#576=B_SPLINE_CURVE_WITH_KNOTS('',3,(#21691,#21692,#21693,#21694,#21695,
#21696,#21697,#21698,#21699,#21700),.UNSPECIFIED.,.F.,.F.,(4,2,2,2,4),(0.528720639901106,
0.611686436801216,0.699059005116263,0.78643157343131,0.869397370331421),
 .UNSPECIFIED.);
#577=B_SPLINE_CURVE_WITH_KNOTS('',3,(#21704,#21705,#21706,#21707,#21708,
#21709,#21710,#21711,#21712,#21713,#21714),.UNSPECIFIED.,.F.,.F.,(4,2,3,
2,4),(-0.170336741191592,-0.0873737681171707,0.,0.0873737681171707,0.170336741191593),
 .UNSPECIFIED.);
#578=B_SPLINE_CURVE_WITH_KNOTS('',3,(#21718,#21719,#21720,#21721,#21722,
#21723,#21724,#21725,#21726,#21727),.UNSPECIFIED.,.F.,.F.,(4,2,2,2,4),(0.528720639901106,
0.611686436801217,0.699059005116263,0.786431573431309,0.86939737033142),
 .UNSPECIFIED.);
#579=B_SPLINE_CURVE_WITH_KNOTS('',3,(#21733,#21734,#21735,#21736,#21737,
#21738),.UNSPECIFIED.,.F.,.F.,(4,2,4),(0.226218361876484,0.259193164726019,
0.292167967575555),.UNSPECIFIED.);
#580=B_SPLINE_CURVE_WITH_KNOTS('',3,(#21739,#21740,#21741,#21742,#21743,
#21744,#21745,#21746,#21747,#21748,#21749),.UNSPECIFIED.,.F.,.F.,(4,2,3,
2,4),(-0.170336741191593,-0.0873737681171707,0.,0.0873737681171706,0.170336741191593),
 .UNSPECIFIED.);
#581=B_SPLINE_CURVE_WITH_KNOTS('',3,(#21751,#21752,#21753,#21754,#21755,
#21756),.UNSPECIFIED.,.F.,.F.,(4,2,4),(0.699168310489759,0.727019400778947,
0.754870491068134),.UNSPECIFIED.);
#582=B_SPLINE_CURVE_WITH_KNOTS('',3,(#21757,#21758,#21759,#21760,#21761,
#21762,#21763,#21764,#21765,#21766),.UNSPECIFIED.,.F.,.F.,(4,2,2,2,4),(0.528720639901106,
0.611686436801216,0.699059005116263,0.786431573431309,0.86939737033142),
 .UNSPECIFIED.);
#583=B_SPLINE_CURVE_WITH_KNOTS('',3,(#21770,#21771,#21772,#21773,#21774,
#21775,#21776,#21777,#21778,#21779,#21780),.UNSPECIFIED.,.F.,.F.,(4,2,3,
2,4),(-0.170336741191592,-0.0873737681171702,0.,0.0873737681171704,0.170336741191593),
 .UNSPECIFIED.);
#584=B_SPLINE_CURVE_WITH_KNOTS('',3,(#21784,#21785,#21786,#21787,#21788,
#21789,#21790,#21791,#21792,#21793),.UNSPECIFIED.,.F.,.F.,(4,2,2,2,4),(0.528720639901106,
0.611686436801217,0.699059005116263,0.78643157343131,0.869397370331421),
 .UNSPECIFIED.);
#585=B_SPLINE_CURVE_WITH_KNOTS('',3,(#21799,#21800,#21801,#21802,#21803,
#21804),.UNSPECIFIED.,.F.,.F.,(4,2,4),(0.226218361876484,0.25919316472602,
0.292167967575555),.UNSPECIFIED.);
#586=B_SPLINE_CURVE_WITH_KNOTS('',3,(#21805,#21806,#21807,#21808,#21809,
#21810,#21811,#21812,#21813,#21814,#21815),.UNSPECIFIED.,.F.,.F.,(4,2,3,
2,4),(-0.170336741191593,-0.0873737681171702,0.,0.0873737681171703,0.170336741191593),
 .UNSPECIFIED.);
#587=B_SPLINE_CURVE_WITH_KNOTS('',3,(#21817,#21818,#21819,#21820,#21821,
#21822),.UNSPECIFIED.,.F.,.F.,(4,2,4),(0.699168310489759,0.727019400778947,
0.754870491068134),.UNSPECIFIED.);
#588=B_SPLINE_CURVE_WITH_KNOTS('',3,(#21823,#21824,#21825,#21826,#21827,
#21828,#21829,#21830,#21831,#21832),.UNSPECIFIED.,.F.,.F.,(4,2,2,2,4),(0.528720639901106,
0.611686436801216,0.699059005116263,0.78643157343131,0.869397370331421),
 .UNSPECIFIED.);
#589=B_SPLINE_CURVE_WITH_KNOTS('',3,(#21836,#21837,#21838,#21839,#21840,
#21841,#21842,#21843,#21844,#21845,#21846),.UNSPECIFIED.,.F.,.F.,(4,2,3,
2,4),(-0.170336741191592,-0.0873737681171707,0.,0.0873737681171707,0.170336741191592),
 .UNSPECIFIED.);
#590=B_SPLINE_CURVE_WITH_KNOTS('',3,(#21850,#21851,#21852,#21853,#21854,
#21855,#21856,#21857,#21858,#21859),.UNSPECIFIED.,.F.,.F.,(4,2,2,2,4),(0.528720639901106,
0.611686436801216,0.699059005116263,0.78643157343131,0.869397370331421),
 .UNSPECIFIED.);
#591=B_SPLINE_CURVE_WITH_KNOTS('',3,(#21865,#21866,#21867,#21868,#21869,
#21870),.UNSPECIFIED.,.F.,.F.,(4,2,4),(0.226218361876484,0.259193164726019,
0.292167967575555),.UNSPECIFIED.);
#592=B_SPLINE_CURVE_WITH_KNOTS('',3,(#21871,#21872,#21873,#21874,#21875,
#21876,#21877,#21878,#21879,#21880,#21881),.UNSPECIFIED.,.F.,.F.,(4,2,3,
2,4),(-0.170336741191592,-0.0873737681171707,0.,0.0873737681171706,0.170336741191593),
 .UNSPECIFIED.);
#593=B_SPLINE_CURVE_WITH_KNOTS('',3,(#21883,#21884,#21885,#21886,#21887,
#21888),.UNSPECIFIED.,.F.,.F.,(4,2,4),(0.69916831048976,0.727019400778947,
0.754870491068134),.UNSPECIFIED.);
#594=B_SPLINE_CURVE_WITH_KNOTS('',3,(#21889,#21890,#21891,#21892,#21893,
#21894,#21895,#21896,#21897,#21898),.UNSPECIFIED.,.F.,.F.,(4,2,2,2,4),(0.528720639901105,
0.611686436801216,0.699059005116263,0.786431573431309,0.86939737033142),
 .UNSPECIFIED.);
#595=B_SPLINE_CURVE_WITH_KNOTS('',3,(#21903,#21904,#21905,#21906,#21907,
#21908),.UNSPECIFIED.,.F.,.F.,(4,2,4),(0.226218361876484,0.259193164726019,
0.292167967575555),.UNSPECIFIED.);
#596=B_SPLINE_CURVE_WITH_KNOTS('',3,(#21914,#21915,#21916,#21917,#21918,
#21919,#21920,#21921,#21922,#21923,#21924),.UNSPECIFIED.,.F.,.F.,(4,2,3,
2,4),(-0.170336741191593,-0.0873737681171707,0.,0.0873737681171706,0.170336741191593),
 .UNSPECIFIED.);
#597=B_SPLINE_CURVE_WITH_KNOTS('',3,(#21932,#21933,#21934,#21935,#21936,
#21937),.UNSPECIFIED.,.F.,.F.,(4,2,4),(0.69916831048976,0.727019400778947,
0.754870491068135),.UNSPECIFIED.);
#598=B_SPLINE_CURVE_WITH_KNOTS('',3,(#21940,#21941,#21942,#21943,#21944,
#21945,#21946,#21947,#21948,#21949),.UNSPECIFIED.,.F.,.F.,(4,2,2,2,4),(0.528720639901106,
0.611686436801216,0.699059005116263,0.78643157343131,0.869397370331421),
 .UNSPECIFIED.);
#599=B_SPLINE_CURVE_WITH_KNOTS('',3,(#21954,#21955,#21956,#21957,#21958,
#21959,#21960,#21961,#21962,#21963),.UNSPECIFIED.,.F.,.F.,(4,2,2,2,4),(0.528720639901106,
0.611686436801217,0.699059005116263,0.78643157343131,0.869397370331421),
 .UNSPECIFIED.);
#600=B_SPLINE_CURVE_WITH_KNOTS('',3,(#21964,#21965,#21966,#21967,#21968,
#21969,#21970,#21971,#21972,#21973,#21974),.UNSPECIFIED.,.F.,.F.,(4,2,3,
2,4),(-0.170336741191593,-0.0873737681171707,0.,0.0873737681171707,0.170336741191593),
 .UNSPECIFIED.);
#601=B_SPLINE_CURVE_WITH_KNOTS('',3,(#22093,#22094,#22095,#22096,#22097,
#22098,#22099,#22100,#22101,#22102),.UNSPECIFIED.,.F.,.F.,(4,3,3,4),(-4.0925417488383,
-3.89049682263533,-2.9178726169765,-2.0651401332781),.UNSPECIFIED.);
#602=B_SPLINE_CURVE_WITH_KNOTS('',3,(#22105,#22106,#22107,#22108,#22109,
#22110,#22111),.UNSPECIFIED.,.F.,.F.,(4,3,4),(0.,0.972624205658834,1.11419103802959),
 .UNSPECIFIED.);
#603=B_SPLINE_CURVE_WITH_KNOTS('',3,(#22116,#22117,#22118,#22119,#22120,
#22121,#22122,#22123,#22124,#22125,#22126,#22127,#22128,#22129,#22130,#22131,
#22132,#22133,#22134,#22135,#22136,#22137),.UNSPECIFIED.,.F.,.F.,(4,3,3,
3,3,3,3,4),(-10.3757270560179,-9.72624205658833,-8.7536178509295,-7.78099364527067,
-6.80836943961183,-5.835745233953,-4.86312102829416,-4.0925417488383),
 .UNSPECIFIED.);
#604=B_SPLINE_CURVE_WITH_KNOTS('',3,(#22138,#22139,#22140,#22141,#22142,
#22143,#22144,#22145,#22146,#22147,#22148,#22149,#22150,#22151,#22152,#22153,
#22154,#22155,#22156,#22157,#22158,#22159),.UNSPECIFIED.,.F.,.F.,(4,3,3,
3,3,3,3,4),(1.11419103802959,1.94524841131767,2.9178726169765,3.89049682263533,
4.86312102829416,5.835745233953,6.80836943961183,7.39737634520917),
 .UNSPECIFIED.);
#605=B_SPLINE_CURVE_WITH_KNOTS('',3,(#22164,#22165,#22166,#22167,#22168,
#22169,#22170,#22171,#22172,#22173,#22174,#22175,#22176,#22177,#22178,#22179,
#22180,#22181,#22182,#22183,#22184,#22185,#22186,#22187,#22188),
 .UNSPECIFIED.,.F.,.F.,(4,3,3,3,3,3,3,3,4),(-16.6589123631975,-16.5346114962002,
-15.5619872905413,-14.5893630848825,-13.6167388792237,-12.6441146735648,
-11.671490467906,-10.6988662622472,-10.3757270560179),.UNSPECIFIED.);
#606=B_SPLINE_CURVE_WITH_KNOTS('',3,(#22189,#22190,#22191,#22192,#22193,
#22194,#22195,#22196,#22197,#22198,#22199,#22200,#22201,#22202,#22203,#22204,
#22205,#22206,#22207,#22208,#22209,#22210,#22211,#22212,#22213),
 .UNSPECIFIED.,.F.,.F.,(4,3,3,3,3,3,3,3,4),(7.39737634520917,7.78099364527067,
8.7536178509295,9.72624205658833,10.6988662622472,11.671490467906,12.6441146735648,
13.6167388792237,13.6805616523888),.UNSPECIFIED.);
#607=B_SPLINE_CURVE_WITH_KNOTS('',3,(#22218,#22219,#22220,#22221,#22222,
#22223,#22224,#22225,#22226,#22227,#22228,#22229,#22230,#22231,#22232,#22233,
#22234,#22235,#22236,#22237,#22238,#22239),.UNSPECIFIED.,.F.,.F.,(4,3,3,
3,3,3,3,4),(-22.9420976703771,-22.3703567301532,-21.3977325244943,-20.4251083188355,
-19.4524841131767,-18.4798599075178,-17.507235701859,-16.6589123631975),
 .UNSPECIFIED.);
#608=B_SPLINE_CURVE_WITH_KNOTS('',3,(#22240,#22241,#22242,#22243,#22244,
#22245,#22246,#22247,#22248,#22249,#22250,#22251,#22252,#22253,#22254,#22255,
#22256,#22257,#22258,#22259,#22260,#22261),.UNSPECIFIED.,.F.,.F.,(4,3,3,
3,3,3,3,4),(13.6805616523888,14.5893630848825,15.5619872905413,16.5346114962002,
17.507235701859,18.4798599075178,19.4524841131767,19.9637469595683),
 .UNSPECIFIED.);
#609=B_SPLINE_CURVE_WITH_KNOTS('',3,(#22266,#22267,#22268,#22269,#22270,
#22271,#22272,#22273,#22274,#22275,#22276,#22277,#22278,#22279,#22280,#22281,
#22282,#22283,#22284,#22285,#22286,#22287,#22288,#22289,#22290),
 .UNSPECIFIED.,.F.,.F.,(4,3,3,3,3,3,3,3,4),(-29.2252829775566,-29.178726169765,
-28.2061019641061,-27.2334777584473,-26.2608535527885,-25.2882293471297,
-24.3156051414708,-23.342980935812,-22.9420976703771),.UNSPECIFIED.);
#610=B_SPLINE_CURVE_WITH_KNOTS('',3,(#22291,#22292,#22293,#22294,#22295,
#22296,#22297,#22298,#22299,#22300,#22301,#22302,#22303,#22304,#22305,#22306,
#22307,#22308,#22309,#22310,#22311,#22312),.UNSPECIFIED.,.F.,.F.,(4,3,3,
3,3,3,3,4),(19.9637469595683,20.4251083188355,21.3977325244943,22.3703567301532,
23.342980935812,24.3156051414708,25.2882293471297,26.2469322667479),
 .UNSPECIFIED.);
#611=B_SPLINE_CURVE_WITH_KNOTS('',3,(#22318,#22319,#22320,#22321,#22322,
#22323,#22324,#22325,#22326,#22327),.UNSPECIFIED.,.F.,.F.,(4,1,1,1,1,1,
1,4),(34.5575191894877,34.9584024549226,35.9310266605815,36.9036508662403,
37.8762750718991,38.848899277558,39.8215234832168,40.6742559669152),
 .UNSPECIFIED.);
#612=B_SPLINE_CURVE_WITH_KNOTS('',3,(#22330,#22331,#22332,#22333,#22334,
#22335,#22336,#22337,#22338),.UNSPECIFIED.,.F.,.F.,(4,1,1,1,1,1,4),(34.5575191894877,
34.5714404755283,35.5440646811871,36.5166888868459,37.4893130925048,38.4619372981636,
39.4345615038224),.UNSPECIFIED.);
#613=B_SPLINE_CURVE_WITH_KNOTS('',3,(#22343,#22344,#22345,#22346,#22347,
#22348,#22349,#22350,#22351,#22352),.UNSPECIFIED.,.F.,.F.,(4,1,1,1,1,1,
1,4),(28.2743338823081,29.1226572209696,30.0952814266285,31.0679056322873,
32.0405298379462,33.013154043605,33.9857782492638,34.5575191894877),
 .UNSPECIFIED.);
#614=B_SPLINE_CURVE_WITH_KNOTS('',3,(#22353,#22354,#22355,#22356,#22357,
#22358,#22359,#22360,#22361,#22362),.UNSPECIFIED.,.F.,.F.,(4,1,1,1,1,1,
1,4),(28.2743338823081,28.7356952415753,29.7083194472341,30.6809436528929,
31.6535678585518,32.6261920642106,33.5988162698694,34.5575191894877),
 .UNSPECIFIED.);
#615=B_SPLINE_CURVE_WITH_KNOTS('',3,(#22367,#22368,#22369,#22370,#22371,
#22372,#22373,#22374,#22375,#22376,#22377),.UNSPECIFIED.,.F.,.F.,(4,1,1,
1,1,1,1,1,4),(21.9911485751285,22.3142877813578,23.2869119870167,24.2595361926755,
25.2321603983343,26.2047846039932,27.177408809652,28.1500330153108,28.2743338823081),
 .UNSPECIFIED.);
#616=B_SPLINE_CURVE_WITH_KNOTS('',3,(#22378,#22379,#22380,#22381,#22382,
#22383,#22384,#22385,#22386,#22387),.UNSPECIFIED.,.F.,.F.,(4,1,1,1,1,1,
1,4),(21.9911485751285,22.8999500076223,23.8725742132811,24.8451984189399,
25.8178226245988,26.7904468302576,27.7630710359164,28.2743338823081),
 .UNSPECIFIED.);
#617=B_SPLINE_CURVE_WITH_KNOTS('',3,(#22392,#22393,#22394,#22395,#22396,
#22397,#22398,#22399,#22400,#22401),.UNSPECIFIED.,.F.,.F.,(4,1,1,1,1,1,
1,4),(15.707963267949,16.4785425474048,17.4511667530637,18.4237909587225,
19.3964151643813,20.3690393700402,21.341663575699,21.9911485751285),
 .UNSPECIFIED.);
#618=B_SPLINE_CURVE_WITH_KNOTS('',3,(#22402,#22403,#22404,#22405,#22406,
#22407,#22408,#22409,#22410,#22411,#22412),.UNSPECIFIED.,.F.,.F.,(4,1,1,
1,1,1,1,1,4),(15.707963267949,16.0915805680104,17.0642047736693,18.0368289793281,
19.0094531849869,19.9820773906458,20.9547015963046,21.9273258019634,21.9911485751285),
 .UNSPECIFIED.);
#619=B_SPLINE_CURVE_WITH_KNOTS('',3,(#22415,#22416,#22417,#22418,#22419,
#22420,#22421,#22422,#22423,#22424,#22425,#22426,#22427,#22428,#22429,#22430,
#22431,#22432,#22433,#22434,#22435,#22436,#22437,#22438,#22439,#22440,#22441,
#22442,#22443,#22444,#22445,#22446,#22447,#22448,#22449,#22450,#22451,#22452,
#22453,#22454,#22455,#22456,#22457,#22458,#22459,#22460,#22461,#22462,#22463,
#22464,#22465,#22466,#22467,#22468,#22469,#22470,#22471,#22472,#22473,#22474,
#22475,#22476,#22477,#22478,#22479,#22480,#22481,#22482,#22483,#22484,#22485,
#22486,#22487,#22488,#22489,#22490,#22491,#22492,#22493,#22494,#22495,#22496,
#22497,#22498,#22499),.UNSPECIFIED.,.F.,.F.,(4,3,3,3,3,3,3,3,3,3,3,3,3,
3,3,3,3,3,3,3,3,3,3,3,3,3,3,3,4),(-0.366397579005846,-0.347363257188953,
-0.329218211863887,-0.325009393505273,-0.321082490381395,-0.302311388689811,
-0.287356752685602,-0.281279336571668,-0.277587132863102,-0.258196137226557,
-0.238390630512147,-0.224461548048146,-0.216308813318665,-0.212872877173384,
-0.192447164346281,-0.182674300656141,-0.162884351200081,-0.152704079250076,
-0.147209531443036,-0.143832357812886,-0.123380863328339,-0.102495295978267,
-0.0814402231007135,-0.0761230417310904,-0.0722380214272327,-0.0506145254855477,
-0.0289263363699853,-0.00767917833856411,0.),.UNSPECIFIED.);
#620=B_SPLINE_CURVE_WITH_KNOTS('',3,(#22504,#22505,#22506,#22507,#22508,
#22509,#22510,#22511,#22512,#22513,#22514,#22515,#22516,#22517,#22518,#22519,
#22520,#22521,#22522,#22523,#22524,#22525,#22526,#22527,#22528,#22529,#22530,
#22531,#22532,#22533,#22534,#22535,#22536,#22537,#22538,#22539,#22540,#22541,
#22542,#22543,#22544,#22545,#22546,#22547,#22548,#22549,#22550,#22551,#22552,
#22553,#22554,#22555,#22556,#22557,#22558,#22559,#22560,#22561,#22562,#22563,
#22564,#22565,#22566,#22567,#22568,#22569,#22570,#22571,#22572,#22573,#22574,
#22575,#22576,#22577,#22578,#22579,#22580,#22581,#22582,#22583,#22584,#22585,
#22586,#22587,#22588,#22589,#22590,#22591,#22592,#22593,#22594),
 .UNSPECIFIED.,.F.,.F.,(4,3,3,3,3,3,3,3,3,3,3,3,3,3,3,3,3,3,3,3,3,3,3,3,
3,3,3,3,3,3,4),(-0.364629307890671,-0.343563547016126,-0.341292769248738,
-0.318859176467321,-0.313664077314457,-0.309555023850011,-0.288248705342857,
-0.272445620549675,-0.266267591248655,-0.261338548959422,-0.240605115981447,
-0.220331301052625,-0.205704482538819,-0.198406645939577,-0.194091633009513,
-0.190312834535266,-0.170732684798973,-0.161824026997401,-0.141596023622726,
-0.132746272146305,-0.127543418016785,-0.12405868853927,-0.104626158396666,
-0.0852389483794393,-0.0662274169672081,-0.0621520251604476,-0.0589039687159043,
-0.0403067180000117,-0.0220368370756797,-0.00434640786838026,0.),
 .UNSPECIFIED.);
#621=B_SPLINE_CURVE_WITH_KNOTS('',3,(#22735,#22736,#22737,#22738,#22739,
#22740,#22741,#22742,#22743,#22744,#22745,#22746,#22747),.UNSPECIFIED.,
 .F.,.F.,(4,3,3,3,4),(26.2469322667479,26.2608535527885,27.2334777584473,
28.2061019641061,29.0588344478045),.UNSPECIFIED.);
#622=B_SPLINE_CURVE_WITH_KNOTS('',3,(#22749,#22750,#22751,#22752,#22753,
#22754,#22755,#22756,#22757,#22758,#22759,#22760,#22761,#22762,#22763,#22764,
#22765,#22766,#22767,#22768,#22769,#22770,#22771,#22772,#22773,#22774,#22775,
#22776,#22777,#22778,#22779,#22780,#22781,#22782,#22783,#22784,#22785,#22786,
#22787,#22788,#22789,#22790,#22791,#22792,#22793,#22794,#22795,#22796,#22797,
#22798,#22799,#22800,#22801,#22802,#22803,#22804,#22805,#22806,#22807,#22808,
#22809,#22810,#22811,#22812,#22813,#22814,#22815,#22816,#22817,#22818,#22819,
#22820,#22821,#22822,#22823,#22824,#22825,#22826,#22827,#22828,#22829,#22830,
#22831,#22832,#22833),.UNSPECIFIED.,.F.,.F.,(4,3,3,3,3,3,3,3,3,3,3,3,3,
3,3,3,3,3,3,3,3,3,3,3,3,3,3,3,4),(-0.36639757900584,-0.347363257188946,
-0.329218191413008,-0.32500933180285,-0.321082398968414,-0.302311278590842,
-0.287356656349004,-0.281279841150401,-0.277587229488243,-0.258196223178148,
-0.23839071719213,-0.224461613058133,-0.21630881282252,-0.212872875022835,
-0.192447163028057,-0.18267430065614,-0.162884341523524,-0.152704070178304,
-0.147209519148588,-0.143832348410372,-0.123380843105627,-0.102495264673586,
-0.0814401902266025,-0.0761229928137137,-0.0722380376448969,-0.0506145340878939,
-0.0289263495480188,-0.00767922076694763,0.),.UNSPECIFIED.);
#623=B_SPLINE_CURVE_WITH_KNOTS('',3,(#22834,#22835,#22836,#22837,#22838,
#22839,#22840,#22841,#22842),.UNSPECIFIED.,.F.,.F.,(4,1,1,1,1,1,4),(10.3757270560179,
11.2284595397163,12.2010837453751,13.173707951034,14.1463321566928,15.1189563623516,
15.707963267949),.UNSPECIFIED.);
#624=B_SPLINE_CURVE_WITH_KNOTS('',3,(#22848,#22849,#22850,#22851,#22852,
#22853,#22854,#22855,#22856,#22857,#22858,#22859,#22860,#22861,#22862,#22863,
#22864,#22865,#22866,#22867,#22868,#22869,#22870,#22871,#22872,#22873,#22874,
#22875,#22876,#22877,#22878,#22879,#22880,#22881,#22882,#22883,#22884,#22885,
#22886,#22887,#22888,#22889,#22890,#22891,#22892,#22893,#22894,#22895,#22896,
#22897,#22898,#22899,#22900,#22901,#22902,#22903,#22904,#22905,#22906,#22907,
#22908,#22909,#22910,#22911,#22912,#22913,#22914,#22915,#22916,#22917,#22918,
#22919,#22920,#22921,#22922,#22923,#22924,#22925,#22926,#22927,#22928,#22929,
#22930,#22931,#22932,#22933,#22934,#22935,#22936,#22937,#22938),
 .UNSPECIFIED.,.F.,.F.,(4,3,3,3,3,3,3,3,3,3,3,3,3,3,3,3,3,3,3,3,3,3,3,3,
3,3,3,3,3,3,4),(-0.364629307890668,-0.343563554406758,-0.341292769248734,
-0.318859176467317,-0.313664088958277,-0.309555028947178,-0.288248710841805,
-0.272445625361255,-0.266267609571851,-0.26133855187035,-0.240605120999503,
-0.220331326646483,-0.205704501734212,-0.198406690155409,-0.194092634197369,
-0.190313011659516,-0.170732881684786,-0.161824026997401,-0.141596023622726,
-0.132746272146305,-0.127543414865392,-0.124058687169216,-0.104626163550009,
-0.0852389404586007,-0.0662273798318025,-0.06215172276271,-0.0589034837300999,
-0.0403062183939592,-0.0220363157458943,-0.00434585567455788,0.),
 .UNSPECIFIED.);
#625=B_SPLINE_CURVE_WITH_KNOTS('',3,(#22941,#22942,#22943,#22944,#22945,
#22946,#22947,#22948),.UNSPECIFIED.,.F.,.F.,(4,1,1,1,1,4),(11.6154215191107,
12.5880457247695,13.5606699304283,14.5332941360872,15.505918341746,15.707963267949),
 .UNSPECIFIED.);
#626=B_SPLINE_CURVE_WITH_KNOTS('',3,(#23089,#23090,#23091,#23092,#23093,
#23094,#23095),.UNSPECIFIED.,.F.,.F.,(4,3,4),(-31.1239745810827,-30.1513503754238,
-29.2252829775566),.UNSPECIFIED.);
#627=SHAPE_REPRESENTATION_RELATIONSHIP('SRR','None',#23300,#637);
#628=SHAPE_REPRESENTATION_RELATIONSHIP('SRR','None',#23301,#638);
#629=SHAPE_REPRESENTATION_RELATIONSHIP('SRR','None',#23302,#639);
#630=SHAPE_REPRESENTATION_RELATIONSHIP('SRR','None',#23303,#640);
#631=SHAPE_REPRESENTATION_RELATIONSHIP('SRR','None',#23304,#641);
#632=SHAPE_REPRESENTATION_RELATIONSHIP('SRR','None',#23305,#642);
#633=SHAPE_REPRESENTATION_RELATIONSHIP('SRR','None',#23306,#643);
#634=SHAPE_REPRESENTATION_RELATIONSHIP('SRR','None',#23307,#644);
#635=SHAPE_REPRESENTATION_RELATIONSHIP('SRR','None',#23308,#645);
#636=SHAPE_REPRESENTATION_RELATIONSHIP('SRR','None',#23309,#646);
#637=ADVANCED_BREP_SHAPE_REPRESENTATION('',(#657),#23244);
#638=ADVANCED_BREP_SHAPE_REPRESENTATION('',(#658),#23245);
#639=ADVANCED_BREP_SHAPE_REPRESENTATION('',(#659),#23246);
#640=ADVANCED_BREP_SHAPE_REPRESENTATION('',(#660),#23247);
#641=ADVANCED_BREP_SHAPE_REPRESENTATION('',(#661),#23248);
#642=ADVANCED_BREP_SHAPE_REPRESENTATION('',(#662),#23249);
#643=ADVANCED_BREP_SHAPE_REPRESENTATION('',(#663),#23250);
#644=ADVANCED_BREP_SHAPE_REPRESENTATION('',(#664),#23251);
#645=ADVANCED_BREP_SHAPE_REPRESENTATION('',(#665),#23252);
#646=ADVANCED_BREP_SHAPE_REPRESENTATION('',(#666),#23253);
#647=STYLED_ITEM('',(#23441),#657);
#648=STYLED_ITEM('',(#23448),#658);
#649=STYLED_ITEM('',(#23455),#659);
#650=STYLED_ITEM('',(#23462),#660);
#651=STYLED_ITEM('',(#23462),#661);
#652=STYLED_ITEM('',(#23462),#662);
#653=STYLED_ITEM('',(#23462),#663);
#654=STYLED_ITEM('',(#23469),#664);
#655=STYLED_ITEM('',(#23469),#665);
#656=STYLED_ITEM('',(#23462),#666);
#657=MANIFOLD_SOLID_BREP('Body1',#7025);
#658=MANIFOLD_SOLID_BREP('Body1',#7026);
#659=MANIFOLD_SOLID_BREP('Body1',#7027);
#660=MANIFOLD_SOLID_BREP('Body1',#7028);
#661=MANIFOLD_SOLID_BREP('Body1',#7029);
#662=MANIFOLD_SOLID_BREP('Body1',#7030);
#663=MANIFOLD_SOLID_BREP('Body1',#7031);
#664=MANIFOLD_SOLID_BREP('Body1',#7032);
#665=MANIFOLD_SOLID_BREP('Body1',#7033);
#666=MANIFOLD_SOLID_BREP('Body1',#7034);
#667=CONICAL_SURFACE('',#7210,19.5,0.785398163397451);
#668=CONICAL_SURFACE('',#7214,1.6,0.785398163397445);
#669=CONICAL_SURFACE('',#7217,1.6,0.785398163397448);
#670=CONICAL_SURFACE('',#7220,1.6,0.785398163397448);
#671=CONICAL_SURFACE('',#7223,1.6,0.785398163397445);
#672=CONICAL_SURFACE('',#7231,1.5,0.785398163397449);
#673=CONICAL_SURFACE('',#7234,1.5,0.785398163397447);
#674=CONICAL_SURFACE('',#7238,1.5,0.785398163397447);
#675=CONICAL_SURFACE('',#7242,1.5,0.785398163397449);
#676=CONICAL_SURFACE('',#7250,3.5,0.785398163397447);
#677=CONICAL_SURFACE('',#7253,3.5,0.785398163397447);
#678=CONICAL_SURFACE('',#7256,3.5,0.785398163397447);
#679=CONICAL_SURFACE('',#7259,3.5,0.785398163397447);
#680=CONICAL_SURFACE('',#7280,12.1473403730037,0.739193465255218);
#681=CONICAL_SURFACE('',#7282,2.175,0.785398163397448);
#682=CONICAL_SURFACE('',#7285,2.175,0.785398163397448);
#683=CONICAL_SURFACE('',#7288,6.275,0.785398163397448);
#684=CONICAL_SURFACE('',#7315,6.275,0.785398163397451);
#685=CONICAL_SURFACE('',#7319,9.75,0.785398163397451);
#686=CONICAL_SURFACE('',#7324,14.5,0.817645045832702);
#687=CONICAL_SURFACE('',#7326,14.5,0.817645045832702);
#688=CONICAL_SURFACE('',#7328,14.5,0.817645045832702);
#689=CONICAL_SURFACE('',#7330,14.5,0.817645045832702);
#690=CONICAL_SURFACE('',#7332,14.5,0.817645045832702);
#691=CONICAL_SURFACE('',#7334,14.5,0.817645045832702);
#692=CONICAL_SURFACE('',#7336,14.5,0.817645045832702);
#693=CONICAL_SURFACE('',#7338,14.5,0.817645045832702);
#694=CONICAL_SURFACE('',#7340,14.5,0.817645045832702);
#695=CONICAL_SURFACE('',#7342,14.5,0.817645045832702);
#696=CONICAL_SURFACE('',#7344,14.5,0.817645045832702);
#697=CONICAL_SURFACE('',#7346,14.5,0.817645045832702);
#698=CONICAL_SURFACE('',#7348,14.5,0.817645045832702);
#699=CONICAL_SURFACE('',#7350,14.5,0.817645045832702);
#700=CONICAL_SURFACE('',#7352,14.5,0.817645045832702);
#701=CONICAL_SURFACE('',#7354,14.5,0.817645045832702);
#702=CONICAL_SURFACE('',#7356,14.5,0.817645045832702);
#703=CONICAL_SURFACE('',#7358,14.5,0.817645045832702);
#704=CONICAL_SURFACE('',#7360,14.5,0.817645045832702);
#705=CONICAL_SURFACE('',#7362,14.5,0.817645045832702);
#706=CONICAL_SURFACE('',#7367,14.5,0.817645045832702);
#707=CONICAL_SURFACE('',#7371,12.1473403730037,0.739193465255218);
#708=CONICAL_SURFACE('',#7413,2.175,0.785398163397448);
#709=CONICAL_SURFACE('',#7416,2.175,0.785398163397448);
#710=CONICAL_SURFACE('',#7419,6.275,0.785398163397448);
#711=CONICAL_SURFACE('',#7447,6.275,0.785398163397451);
#712=CONICAL_SURFACE('',#7451,9.75,0.785398163397451);
#713=CONICAL_SURFACE('',#7456,14.5,0.817645045832702);
#714=CONICAL_SURFACE('',#7458,14.5,0.817645045832702);
#715=CONICAL_SURFACE('',#7460,14.5,0.817645045832702);
#716=CONICAL_SURFACE('',#7462,14.5,0.817645045832702);
#717=CONICAL_SURFACE('',#7464,14.5,0.817645045832702);
#718=CONICAL_SURFACE('',#7466,14.5,0.817645045832702);
#719=CONICAL_SURFACE('',#7468,14.5,0.817645045832702);
#720=CONICAL_SURFACE('',#7470,14.5,0.817645045832702);
#721=CONICAL_SURFACE('',#7472,14.5,0.817645045832702);
#722=CONICAL_SURFACE('',#7474,14.5,0.817645045832702);
#723=CONICAL_SURFACE('',#7476,14.5,0.817645045832702);
#724=CONICAL_SURFACE('',#7478,14.5,0.817645045832702);
#725=CONICAL_SURFACE('',#7480,14.5,0.817645045832702);
#726=CONICAL_SURFACE('',#7482,14.5,0.817645045832702);
#727=CONICAL_SURFACE('',#7484,14.5,0.817645045832702);
#728=CONICAL_SURFACE('',#7486,14.5,0.817645045832702);
#729=CONICAL_SURFACE('',#7488,14.5,0.817645045832702);
#730=CONICAL_SURFACE('',#7490,14.5,0.817645045832702);
#731=CONICAL_SURFACE('',#7492,14.5,0.817645045832702);
#732=CONICAL_SURFACE('',#7494,14.5,0.817645045832702);
#733=CONICAL_SURFACE('',#7499,14.5,0.817645045832702);
#734=CONICAL_SURFACE('',#7503,12.1473403730037,0.739193465255218);
#735=CONICAL_SURFACE('',#7557,0.625,1.04746029293308);
#736=CONICAL_SURFACE('',#7564,1.25,1.04746029293308);
#737=CONICAL_SURFACE('',#7567,5.6,0.785398163397448);
#738=CONICAL_SURFACE('',#7571,5.6,0.785398163397448);
#739=CONICAL_SURFACE('',#7587,0.625,1.04746029293308);
#740=CONICAL_SURFACE('',#7594,1.25,1.04746029293308);
#741=CONICAL_SURFACE('',#7597,5.6,0.785398163397448);
#742=CONICAL_SURFACE('',#7601,5.6,0.785398163397448);
#743=CONICAL_SURFACE('',#7607,12.15,1.01175638808434);
#744=CONICAL_SURFACE('',#7694,13.85,0.785398163397449);
#745=CONICAL_SURFACE('',#7698,13.85,0.785398163397448);
#746=CONICAL_SURFACE('',#7706,6.15,0.785398163397448);
#747=CONICAL_SURFACE('',#7710,6.15,0.785398163397449);
#748=CONICAL_SURFACE('',#7717,8.55,0.643501108793281);
#749=CONICAL_SURFACE('',#7721,11.65,0.643501108793288);
#750=CONICAL_SURFACE('',#7725,13.85,0.785398163397449);
#751=CONICAL_SURFACE('',#7729,13.85,0.785398163397448);
#752=CONICAL_SURFACE('',#7733,11.65,0.643501108793288);
#753=CONICAL_SURFACE('',#7737,8.55,0.643501108793281);
#754=CONICAL_SURFACE('',#7741,6.15,0.785398163397448);
#755=CONICAL_SURFACE('',#7745,6.15,0.785398163397449);
#756=CONICAL_SURFACE('',#7775,0.5,1.02305631307899);
#757=CONICAL_SURFACE('',#7786,1.75,0.83798122500839);
#758=CONICAL_SURFACE('',#7789,1.8,0.785398163397448);
#759=TOROIDAL_SURFACE('',#7197,21.5,1.5);
#760=TOROIDAL_SURFACE('',#7619,10.,2.36);
#761=TOROIDAL_SURFACE('',#7633,10.,2.36);
#762=TOROIDAL_SURFACE('',#7637,10.,2.36);
#763=TOROIDAL_SURFACE('',#7639,10.,2.36);
#764=TOROIDAL_SURFACE('',#7643,10.,2.36);
#765=TOROIDAL_SURFACE('',#7645,10.,2.36);
#766=TOROIDAL_SURFACE('',#7649,10.,2.36);
#767=TOROIDAL_SURFACE('',#7651,10.,2.36);
#768=TOROIDAL_SURFACE('',#7655,10.,2.36);
#769=TOROIDAL_SURFACE('',#7657,10.,2.36);
#770=TOROIDAL_SURFACE('',#7661,10.,2.36);
#771=TOROIDAL_SURFACE('',#7663,10.,2.36);
#772=TOROIDAL_SURFACE('',#7667,10.,2.36);
#773=TOROIDAL_SURFACE('',#7669,10.,2.36);
#774=TOROIDAL_SURFACE('',#7673,10.,2.36);
#775=TOROIDAL_SURFACE('',#7675,10.,2.36);
#776=TOROIDAL_SURFACE('',#7683,10.,2.36);
#777=TOROIDAL_SURFACE('',#7688,10.,2.36);
#778=TOROIDAL_SURFACE('',#7691,10.,2.36);
#779=TOROIDAL_SURFACE('',#7703,10.,2.36);
#780=FACE_BOUND('',#1376,.T.);
#781=FACE_BOUND('',#1379,.T.);
#782=FACE_BOUND('',#1382,.T.);
#783=FACE_BOUND('',#1385,.T.);
#784=FACE_BOUND('',#1389,.T.);
#785=FACE_BOUND('',#1392,.T.);
#786=FACE_BOUND('',#1395,.T.);
#787=FACE_BOUND('',#1399,.T.);
#788=FACE_BOUND('',#1402,.T.);
#789=FACE_BOUND('',#1405,.T.);
#790=FACE_BOUND('',#1410,.T.);
#791=FACE_BOUND('',#1413,.T.);
#792=FACE_BOUND('',#1424,.T.);
#793=FACE_BOUND('',#1436,.T.);
#794=FACE_BOUND('',#1446,.T.);
#795=FACE_BOUND('',#1451,.T.);
#796=FACE_BOUND('',#1453,.T.);
#797=FACE_BOUND('',#1459,.T.);
#798=FACE_BOUND('',#1469,.T.);
#799=FACE_BOUND('',#1471,.T.);
#800=FACE_BOUND('',#1474,.T.);
#801=FACE_BOUND('',#1477,.T.);
#802=FACE_BOUND('',#1562,.T.);
#803=FACE_BOUND('',#1569,.T.);
#804=FACE_BOUND('',#1571,.T.);
#805=FACE_BOUND('',#1574,.T.);
#806=FACE_BOUND('',#1577,.T.);
#807=FACE_BOUND('',#1662,.T.);
#808=FACE_BOUND('',#1674,.T.);
#809=FACE_BOUND('',#1677,.T.);
#810=FACE_BOUND('',#1680,.T.);
#811=FACE_BOUND('',#1692,.T.);
#812=FACE_BOUND('',#1695,.T.);
#813=FACE_BOUND('',#1698,.T.);
#814=FACE_BOUND('',#1700,.T.);
#815=FACE_BOUND('',#1701,.T.);
#816=FACE_BOUND('',#1707,.T.);
#817=FACE_BOUND('',#1708,.T.);
#818=FACE_BOUND('',#1712,.T.);
#819=FACE_BOUND('',#1713,.T.);
#820=FACE_BOUND('',#1717,.T.);
#821=FACE_BOUND('',#1718,.T.);
#822=FACE_BOUND('',#1722,.T.);
#823=FACE_BOUND('',#1723,.T.);
#824=FACE_BOUND('',#1727,.T.);
#825=FACE_BOUND('',#1728,.T.);
#826=FACE_BOUND('',#1732,.T.);
#827=FACE_BOUND('',#1733,.T.);
#828=FACE_BOUND('',#1737,.T.);
#829=FACE_BOUND('',#1738,.T.);
#830=FACE_BOUND('',#1742,.T.);
#831=FACE_BOUND('',#1743,.T.);
#832=FACE_BOUND('',#1749,.T.);
#833=FACE_BOUND('',#1750,.T.);
#834=FACE_BOUND('',#1753,.T.);
#835=FACE_BOUND('',#1758,.T.);
#836=FACE_BOUND('',#1762,.T.);
#837=FACE_BOUND('',#1767,.T.);
#838=FACE_BOUND('',#1769,.T.);
#839=FACE_BOUND('',#1772,.T.);
#840=FACE_BOUND('',#1775,.T.);
#841=FACE_BOUND('',#1780,.T.);
#842=FACE_BOUND('',#1783,.T.);
#843=FACE_BOUND('',#1786,.T.);
#844=FACE_BOUND('',#1792,.T.);
#845=FACE_BOUND('',#1795,.T.);
#846=FACE_BOUND('',#1818,.T.);
#847=FACE_BOUND('',#1824,.T.);
#848=FACE_BOUND('',#1829,.T.);
#849=FACE_BOUND('',#1830,.T.);
#850=FACE_BOUND('',#1838,.T.);
#851=FACE_BOUND('',#1839,.T.);
#852=PLANE('',#7151);
#853=PLANE('',#7155);
#854=PLANE('',#7159);
#855=PLANE('',#7163);
#856=PLANE('',#7170);
#857=PLANE('',#7174);
#858=PLANE('',#7178);
#859=PLANE('',#7185);
#860=PLANE('',#7189);
#861=PLANE('',#7193);
#862=PLANE('',#7205);
#863=PLANE('',#7212);
#864=PLANE('',#7213);
#865=PLANE('',#7216);
#866=PLANE('',#7219);
#867=PLANE('',#7222);
#868=PLANE('',#7227);
#869=PLANE('',#7230);
#870=PLANE('',#7233);
#871=PLANE('',#7237);
#872=PLANE('',#7241);
#873=PLANE('',#7244);
#874=PLANE('',#7245);
#875=PLANE('',#7252);
#876=PLANE('',#7255);
#877=PLANE('',#7258);
#878=PLANE('',#7261);
#879=PLANE('',#7262);
#880=PLANE('',#7265);
#881=PLANE('',#7268);
#882=PLANE('',#7271);
#883=PLANE('',#7274);
#884=PLANE('',#7276);
#885=PLANE('',#7278);
#886=PLANE('',#7295);
#887=PLANE('',#7317);
#888=PLANE('',#7369);
#889=PLANE('',#7392);
#890=PLANE('',#7393);
#891=PLANE('',#7394);
#892=PLANE('',#7395);
#893=PLANE('',#7396);
#894=PLANE('',#7397);
#895=PLANE('',#7398);
#896=PLANE('',#7399);
#897=PLANE('',#7400);
#898=PLANE('',#7401);
#899=PLANE('',#7402);
#900=PLANE('',#7403);
#901=PLANE('',#7404);
#902=PLANE('',#7405);
#903=PLANE('',#7406);
#904=PLANE('',#7407);
#905=PLANE('',#7408);
#906=PLANE('',#7409);
#907=PLANE('',#7410);
#908=PLANE('',#7411);
#909=PLANE('',#7426);
#910=PLANE('',#7449);
#911=PLANE('',#7501);
#912=PLANE('',#7524);
#913=PLANE('',#7525);
#914=PLANE('',#7526);
#915=PLANE('',#7527);
#916=PLANE('',#7528);
#917=PLANE('',#7529);
#918=PLANE('',#7530);
#919=PLANE('',#7531);
#920=PLANE('',#7532);
#921=PLANE('',#7533);
#922=PLANE('',#7534);
#923=PLANE('',#7535);
#924=PLANE('',#7536);
#925=PLANE('',#7537);
#926=PLANE('',#7538);
#927=PLANE('',#7539);
#928=PLANE('',#7540);
#929=PLANE('',#7541);
#930=PLANE('',#7542);
#931=PLANE('',#7543);
#932=PLANE('',#7545);
#933=PLANE('',#7548);
#934=PLANE('',#7551);
#935=PLANE('',#7552);
#936=PLANE('',#7554);
#937=PLANE('',#7555);
#938=PLANE('',#7565);
#939=PLANE('',#7573);
#940=PLANE('',#7575);
#941=PLANE('',#7578);
#942=PLANE('',#7581);
#943=PLANE('',#7582);
#944=PLANE('',#7584);
#945=PLANE('',#7585);
#946=PLANE('',#7595);
#947=PLANE('',#7603);
#948=PLANE('',#7692);
#949=PLANE('',#7700);
#950=PLANE('',#7704);
#951=PLANE('',#7712);
#952=PLANE('',#7714);
#953=PLANE('',#7719);
#954=PLANE('',#7723);
#955=PLANE('',#7731);
#956=PLANE('',#7735);
#957=PLANE('',#7739);
#958=PLANE('',#7750);
#959=PLANE('',#7754);
#960=PLANE('',#7767);
#961=PLANE('',#7770);
#962=PLANE('',#7777);
#963=PLANE('',#7778);
#964=PLANE('',#7779);
#965=PLANE('',#7780);
#966=PLANE('',#7781);
#967=PLANE('',#7782);
#968=PLANE('',#7783);
#969=PLANE('',#7784);
#970=PLANE('',#7791);
#971=PLANE('',#7802);
#972=PLANE('',#7804);
#973=PLANE('',#7805);
#974=PLANE('',#7806);
#975=PLANE('',#7807);
#976=PLANE('',#7808);
#977=PLANE('',#7809);
#978=PLANE('',#7810);
#979=FACE_OUTER_BOUND('',#1374,.T.);
#980=FACE_OUTER_BOUND('',#1375,.T.);
#981=FACE_OUTER_BOUND('',#1377,.T.);
#982=FACE_OUTER_BOUND('',#1378,.T.);
#983=FACE_OUTER_BOUND('',#1380,.T.);
#984=FACE_OUTER_BOUND('',#1381,.T.);
#985=FACE_OUTER_BOUND('',#1383,.T.);
#986=FACE_OUTER_BOUND('',#1384,.T.);
#987=FACE_OUTER_BOUND('',#1386,.T.);
#988=FACE_OUTER_BOUND('',#1387,.T.);
#989=FACE_OUTER_BOUND('',#1388,.T.);
#990=FACE_OUTER_BOUND('',#1390,.T.);
#991=FACE_OUTER_BOUND('',#1391,.T.);
#992=FACE_OUTER_BOUND('',#1393,.T.);
#993=FACE_OUTER_BOUND('',#1394,.T.);
#994=FACE_OUTER_BOUND('',#1396,.T.);
#995=FACE_OUTER_BOUND('',#1397,.T.);
#996=FACE_OUTER_BOUND('',#1398,.T.);
#997=FACE_OUTER_BOUND('',#1400,.T.);
#998=FACE_OUTER_BOUND('',#1401,.T.);
#999=FACE_OUTER_BOUND('',#1403,.T.);
#1000=FACE_OUTER_BOUND('',#1404,.T.);
#1001=FACE_OUTER_BOUND('',#1406,.T.);
#1002=FACE_OUTER_BOUND('',#1407,.T.);
#1003=FACE_OUTER_BOUND('',#1408,.T.);
#1004=FACE_OUTER_BOUND('',#1409,.T.);
#1005=FACE_OUTER_BOUND('',#1411,.T.);
#1006=FACE_OUTER_BOUND('',#1412,.T.);
#1007=FACE_OUTER_BOUND('',#1414,.T.);
#1008=FACE_OUTER_BOUND('',#1415,.T.);
#1009=FACE_OUTER_BOUND('',#1416,.T.);
#1010=FACE_OUTER_BOUND('',#1417,.T.);
#1011=FACE_OUTER_BOUND('',#1418,.T.);
#1012=FACE_OUTER_BOUND('',#1419,.T.);
#1013=FACE_OUTER_BOUND('',#1420,.T.);
#1014=FACE_OUTER_BOUND('',#1421,.T.);
#1015=FACE_OUTER_BOUND('',#1422,.T.);
#1016=FACE_OUTER_BOUND('',#1423,.T.);
#1017=FACE_OUTER_BOUND('',#1425,.T.);
#1018=FACE_OUTER_BOUND('',#1426,.T.);
#1019=FACE_OUTER_BOUND('',#1427,.T.);
#1020=FACE_OUTER_BOUND('',#1428,.T.);
#1021=FACE_OUTER_BOUND('',#1429,.T.);
#1022=FACE_OUTER_BOUND('',#1430,.T.);
#1023=FACE_OUTER_BOUND('',#1431,.T.);
#1024=FACE_OUTER_BOUND('',#1432,.T.);
#1025=FACE_OUTER_BOUND('',#1433,.T.);
#1026=FACE_OUTER_BOUND('',#1434,.T.);
#1027=FACE_OUTER_BOUND('',#1435,.T.);
#1028=FACE_OUTER_BOUND('',#1437,.T.);
#1029=FACE_OUTER_BOUND('',#1438,.T.);
#1030=FACE_OUTER_BOUND('',#1439,.T.);
#1031=FACE_OUTER_BOUND('',#1440,.T.);
#1032=FACE_OUTER_BOUND('',#1441,.T.);
#1033=FACE_OUTER_BOUND('',#1442,.T.);
#1034=FACE_OUTER_BOUND('',#1443,.T.);
#1035=FACE_OUTER_BOUND('',#1444,.T.);
#1036=FACE_OUTER_BOUND('',#1445,.T.);
#1037=FACE_OUTER_BOUND('',#1447,.T.);
#1038=FACE_OUTER_BOUND('',#1448,.T.);
#1039=FACE_OUTER_BOUND('',#1449,.T.);
#1040=FACE_OUTER_BOUND('',#1450,.T.);
#1041=FACE_OUTER_BOUND('',#1452,.T.);
#1042=FACE_OUTER_BOUND('',#1454,.T.);
#1043=FACE_OUTER_BOUND('',#1455,.T.);
#1044=FACE_OUTER_BOUND('',#1456,.T.);
#1045=FACE_OUTER_BOUND('',#1457,.T.);
#1046=FACE_OUTER_BOUND('',#1458,.T.);
#1047=FACE_OUTER_BOUND('',#1460,.T.);
#1048=FACE_OUTER_BOUND('',#1461,.T.);
#1049=FACE_OUTER_BOUND('',#1462,.T.);
#1050=FACE_OUTER_BOUND('',#1463,.T.);
#1051=FACE_OUTER_BOUND('',#1464,.T.);
#1052=FACE_OUTER_BOUND('',#1465,.T.);
#1053=FACE_OUTER_BOUND('',#1466,.T.);
#1054=FACE_OUTER_BOUND('',#1467,.T.);
#1055=FACE_OUTER_BOUND('',#1468,.T.);
#1056=FACE_OUTER_BOUND('',#1470,.T.);
#1057=FACE_OUTER_BOUND('',#1472,.T.);
#1058=FACE_OUTER_BOUND('',#1473,.T.);
#1059=FACE_OUTER_BOUND('',#1475,.T.);
#1060=FACE_OUTER_BOUND('',#1476,.T.);
#1061=FACE_OUTER_BOUND('',#1478,.T.);
#1062=FACE_OUTER_BOUND('',#1479,.T.);
#1063=FACE_OUTER_BOUND('',#1480,.T.);
#1064=FACE_OUTER_BOUND('',#1481,.T.);
#1065=FACE_OUTER_BOUND('',#1482,.T.);
#1066=FACE_OUTER_BOUND('',#1483,.T.);
#1067=FACE_OUTER_BOUND('',#1484,.T.);
#1068=FACE_OUTER_BOUND('',#1485,.T.);
#1069=FACE_OUTER_BOUND('',#1486,.T.);
#1070=FACE_OUTER_BOUND('',#1487,.T.);
#1071=FACE_OUTER_BOUND('',#1488,.T.);
#1072=FACE_OUTER_BOUND('',#1489,.T.);
#1073=FACE_OUTER_BOUND('',#1490,.T.);
#1074=FACE_OUTER_BOUND('',#1491,.T.);
#1075=FACE_OUTER_BOUND('',#1492,.T.);
#1076=FACE_OUTER_BOUND('',#1493,.T.);
#1077=FACE_OUTER_BOUND('',#1494,.T.);
#1078=FACE_OUTER_BOUND('',#1495,.T.);
#1079=FACE_OUTER_BOUND('',#1496,.T.);
#1080=FACE_OUTER_BOUND('',#1497,.T.);
#1081=FACE_OUTER_BOUND('',#1498,.T.);
#1082=FACE_OUTER_BOUND('',#1499,.T.);
#1083=FACE_OUTER_BOUND('',#1500,.T.);
#1084=FACE_OUTER_BOUND('',#1501,.T.);
#1085=FACE_OUTER_BOUND('',#1502,.T.);
#1086=FACE_OUTER_BOUND('',#1503,.T.);
#1087=FACE_OUTER_BOUND('',#1504,.T.);
#1088=FACE_OUTER_BOUND('',#1505,.T.);
#1089=FACE_OUTER_BOUND('',#1506,.T.);
#1090=FACE_OUTER_BOUND('',#1507,.T.);
#1091=FACE_OUTER_BOUND('',#1508,.T.);
#1092=FACE_OUTER_BOUND('',#1509,.T.);
#1093=FACE_OUTER_BOUND('',#1510,.T.);
#1094=FACE_OUTER_BOUND('',#1511,.T.);
#1095=FACE_OUTER_BOUND('',#1512,.T.);
#1096=FACE_OUTER_BOUND('',#1513,.T.);
#1097=FACE_OUTER_BOUND('',#1514,.T.);
#1098=FACE_OUTER_BOUND('',#1515,.T.);
#1099=FACE_OUTER_BOUND('',#1516,.T.);
#1100=FACE_OUTER_BOUND('',#1517,.T.);
#1101=FACE_OUTER_BOUND('',#1518,.T.);
#1102=FACE_OUTER_BOUND('',#1519,.T.);
#1103=FACE_OUTER_BOUND('',#1520,.T.);
#1104=FACE_OUTER_BOUND('',#1521,.T.);
#1105=FACE_OUTER_BOUND('',#1522,.T.);
#1106=FACE_OUTER_BOUND('',#1523,.T.);
#1107=FACE_OUTER_BOUND('',#1524,.T.);
#1108=FACE_OUTER_BOUND('',#1525,.T.);
#1109=FACE_OUTER_BOUND('',#1526,.T.);
#1110=FACE_OUTER_BOUND('',#1527,.T.);
#1111=FACE_OUTER_BOUND('',#1528,.T.);
#1112=FACE_OUTER_BOUND('',#1529,.T.);
#1113=FACE_OUTER_BOUND('',#1530,.T.);
#1114=FACE_OUTER_BOUND('',#1531,.T.);
#1115=FACE_OUTER_BOUND('',#1532,.T.);
#1116=FACE_OUTER_BOUND('',#1533,.T.);
#1117=FACE_OUTER_BOUND('',#1534,.T.);
#1118=FACE_OUTER_BOUND('',#1535,.T.);
#1119=FACE_OUTER_BOUND('',#1536,.T.);
#1120=FACE_OUTER_BOUND('',#1537,.T.);
#1121=FACE_OUTER_BOUND('',#1538,.T.);
#1122=FACE_OUTER_BOUND('',#1539,.T.);
#1123=FACE_OUTER_BOUND('',#1540,.T.);
#1124=FACE_OUTER_BOUND('',#1541,.T.);
#1125=FACE_OUTER_BOUND('',#1542,.T.);
#1126=FACE_OUTER_BOUND('',#1543,.T.);
#1127=FACE_OUTER_BOUND('',#1544,.T.);
#1128=FACE_OUTER_BOUND('',#1545,.T.);
#1129=FACE_OUTER_BOUND('',#1546,.T.);
#1130=FACE_OUTER_BOUND('',#1547,.T.);
#1131=FACE_OUTER_BOUND('',#1548,.T.);
#1132=FACE_OUTER_BOUND('',#1549,.T.);
#1133=FACE_OUTER_BOUND('',#1550,.T.);
#1134=FACE_OUTER_BOUND('',#1551,.T.);
#1135=FACE_OUTER_BOUND('',#1552,.T.);
#1136=FACE_OUTER_BOUND('',#1553,.T.);
#1137=FACE_OUTER_BOUND('',#1554,.T.);
#1138=FACE_OUTER_BOUND('',#1555,.T.);
#1139=FACE_OUTER_BOUND('',#1556,.T.);
#1140=FACE_OUTER_BOUND('',#1557,.T.);
#1141=FACE_OUTER_BOUND('',#1558,.T.);
#1142=FACE_OUTER_BOUND('',#1559,.T.);
#1143=FACE_OUTER_BOUND('',#1560,.T.);
#1144=FACE_OUTER_BOUND('',#1561,.T.);
#1145=FACE_OUTER_BOUND('',#1563,.T.);
#1146=FACE_OUTER_BOUND('',#1564,.T.);
#1147=FACE_OUTER_BOUND('',#1565,.T.);
#1148=FACE_OUTER_BOUND('',#1566,.T.);
#1149=FACE_OUTER_BOUND('',#1567,.T.);
#1150=FACE_OUTER_BOUND('',#1568,.T.);
#1151=FACE_OUTER_BOUND('',#1570,.T.);
#1152=FACE_OUTER_BOUND('',#1572,.T.);
#1153=FACE_OUTER_BOUND('',#1573,.T.);
#1154=FACE_OUTER_BOUND('',#1575,.T.);
#1155=FACE_OUTER_BOUND('',#1576,.T.);
#1156=FACE_OUTER_BOUND('',#1578,.T.);
#1157=FACE_OUTER_BOUND('',#1579,.T.);
#1158=FACE_OUTER_BOUND('',#1580,.T.);
#1159=FACE_OUTER_BOUND('',#1581,.T.);
#1160=FACE_OUTER_BOUND('',#1582,.T.);
#1161=FACE_OUTER_BOUND('',#1583,.T.);
#1162=FACE_OUTER_BOUND('',#1584,.T.);
#1163=FACE_OUTER_BOUND('',#1585,.T.);
#1164=FACE_OUTER_BOUND('',#1586,.T.);
#1165=FACE_OUTER_BOUND('',#1587,.T.);
#1166=FACE_OUTER_BOUND('',#1588,.T.);
#1167=FACE_OUTER_BOUND('',#1589,.T.);
#1168=FACE_OUTER_BOUND('',#1590,.T.);
#1169=FACE_OUTER_BOUND('',#1591,.T.);
#1170=FACE_OUTER_BOUND('',#1592,.T.);
#1171=FACE_OUTER_BOUND('',#1593,.T.);
#1172=FACE_OUTER_BOUND('',#1594,.T.);
#1173=FACE_OUTER_BOUND('',#1595,.T.);
#1174=FACE_OUTER_BOUND('',#1596,.T.);
#1175=FACE_OUTER_BOUND('',#1597,.T.);
#1176=FACE_OUTER_BOUND('',#1598,.T.);
#1177=FACE_OUTER_BOUND('',#1599,.T.);
#1178=FACE_OUTER_BOUND('',#1600,.T.);
#1179=FACE_OUTER_BOUND('',#1601,.T.);
#1180=FACE_OUTER_BOUND('',#1602,.T.);
#1181=FACE_OUTER_BOUND('',#1603,.T.);
#1182=FACE_OUTER_BOUND('',#1604,.T.);
#1183=FACE_OUTER_BOUND('',#1605,.T.);
#1184=FACE_OUTER_BOUND('',#1606,.T.);
#1185=FACE_OUTER_BOUND('',#1607,.T.);
#1186=FACE_OUTER_BOUND('',#1608,.T.);
#1187=FACE_OUTER_BOUND('',#1609,.T.);
#1188=FACE_OUTER_BOUND('',#1610,.T.);
#1189=FACE_OUTER_BOUND('',#1611,.T.);
#1190=FACE_OUTER_BOUND('',#1612,.T.);
#1191=FACE_OUTER_BOUND('',#1613,.T.);
#1192=FACE_OUTER_BOUND('',#1614,.T.);
#1193=FACE_OUTER_BOUND('',#1615,.T.);
#1194=FACE_OUTER_BOUND('',#1616,.T.);
#1195=FACE_OUTER_BOUND('',#1617,.T.);
#1196=FACE_OUTER_BOUND('',#1618,.T.);
#1197=FACE_OUTER_BOUND('',#1619,.T.);
#1198=FACE_OUTER_BOUND('',#1620,.T.);
#1199=FACE_OUTER_BOUND('',#1621,.T.);
#1200=FACE_OUTER_BOUND('',#1622,.T.);
#1201=FACE_OUTER_BOUND('',#1623,.T.);
#1202=FACE_OUTER_BOUND('',#1624,.T.);
#1203=FACE_OUTER_BOUND('',#1625,.T.);
#1204=FACE_OUTER_BOUND('',#1626,.T.);
#1205=FACE_OUTER_BOUND('',#1627,.T.);
#1206=FACE_OUTER_BOUND('',#1628,.T.);
#1207=FACE_OUTER_BOUND('',#1629,.T.);
#1208=FACE_OUTER_BOUND('',#1630,.T.);
#1209=FACE_OUTER_BOUND('',#1631,.T.);
#1210=FACE_OUTER_BOUND('',#1632,.T.);
#1211=FACE_OUTER_BOUND('',#1633,.T.);
#1212=FACE_OUTER_BOUND('',#1634,.T.);
#1213=FACE_OUTER_BOUND('',#1635,.T.);
#1214=FACE_OUTER_BOUND('',#1636,.T.);
#1215=FACE_OUTER_BOUND('',#1637,.T.);
#1216=FACE_OUTER_BOUND('',#1638,.T.);
#1217=FACE_OUTER_BOUND('',#1639,.T.);
#1218=FACE_OUTER_BOUND('',#1640,.T.);
#1219=FACE_OUTER_BOUND('',#1641,.T.);
#1220=FACE_OUTER_BOUND('',#1642,.T.);
#1221=FACE_OUTER_BOUND('',#1643,.T.);
#1222=FACE_OUTER_BOUND('',#1644,.T.);
#1223=FACE_OUTER_BOUND('',#1645,.T.);
#1224=FACE_OUTER_BOUND('',#1646,.T.);
#1225=FACE_OUTER_BOUND('',#1647,.T.);
#1226=FACE_OUTER_BOUND('',#1648,.T.);
#1227=FACE_OUTER_BOUND('',#1649,.T.);
#1228=FACE_OUTER_BOUND('',#1650,.T.);
#1229=FACE_OUTER_BOUND('',#1651,.T.);
#1230=FACE_OUTER_BOUND('',#1652,.T.);
#1231=FACE_OUTER_BOUND('',#1653,.T.);
#1232=FACE_OUTER_BOUND('',#1654,.T.);
#1233=FACE_OUTER_BOUND('',#1655,.T.);
#1234=FACE_OUTER_BOUND('',#1656,.T.);
#1235=FACE_OUTER_BOUND('',#1657,.T.);
#1236=FACE_OUTER_BOUND('',#1658,.T.);
#1237=FACE_OUTER_BOUND('',#1659,.T.);
#1238=FACE_OUTER_BOUND('',#1660,.T.);
#1239=FACE_OUTER_BOUND('',#1661,.T.);
#1240=FACE_OUTER_BOUND('',#1663,.T.);
#1241=FACE_OUTER_BOUND('',#1664,.T.);
#1242=FACE_OUTER_BOUND('',#1665,.T.);
#1243=FACE_OUTER_BOUND('',#1666,.T.);
#1244=FACE_OUTER_BOUND('',#1667,.T.);
#1245=FACE_OUTER_BOUND('',#1668,.T.);
#1246=FACE_OUTER_BOUND('',#1669,.T.);
#1247=FACE_OUTER_BOUND('',#1670,.T.);
#1248=FACE_OUTER_BOUND('',#1671,.T.);
#1249=FACE_OUTER_BOUND('',#1672,.T.);
#1250=FACE_OUTER_BOUND('',#1673,.T.);
#1251=FACE_OUTER_BOUND('',#1675,.T.);
#1252=FACE_OUTER_BOUND('',#1676,.T.);
#1253=FACE_OUTER_BOUND('',#1678,.T.);
#1254=FACE_OUTER_BOUND('',#1679,.T.);
#1255=FACE_OUTER_BOUND('',#1681,.T.);
#1256=FACE_OUTER_BOUND('',#1682,.T.);
#1257=FACE_OUTER_BOUND('',#1683,.T.);
#1258=FACE_OUTER_BOUND('',#1684,.T.);
#1259=FACE_OUTER_BOUND('',#1685,.T.);
#1260=FACE_OUTER_BOUND('',#1686,.T.);
#1261=FACE_OUTER_BOUND('',#1687,.T.);
#1262=FACE_OUTER_BOUND('',#1688,.T.);
#1263=FACE_OUTER_BOUND('',#1689,.T.);
#1264=FACE_OUTER_BOUND('',#1690,.T.);
#1265=FACE_OUTER_BOUND('',#1691,.T.);
#1266=FACE_OUTER_BOUND('',#1693,.T.);
#1267=FACE_OUTER_BOUND('',#1694,.T.);
#1268=FACE_OUTER_BOUND('',#1696,.T.);
#1269=FACE_OUTER_BOUND('',#1697,.T.);
#1270=FACE_OUTER_BOUND('',#1699,.T.);
#1271=FACE_OUTER_BOUND('',#1702,.T.);
#1272=FACE_OUTER_BOUND('',#1703,.T.);
#1273=FACE_OUTER_BOUND('',#1704,.T.);
#1274=FACE_OUTER_BOUND('',#1705,.T.);
#1275=FACE_OUTER_BOUND('',#1706,.T.);
#1276=FACE_OUTER_BOUND('',#1709,.T.);
#1277=FACE_OUTER_BOUND('',#1710,.T.);
#1278=FACE_OUTER_BOUND('',#1711,.T.);
#1279=FACE_OUTER_BOUND('',#1714,.T.);
#1280=FACE_OUTER_BOUND('',#1715,.T.);
#1281=FACE_OUTER_BOUND('',#1716,.T.);
#1282=FACE_OUTER_BOUND('',#1719,.T.);
#1283=FACE_OUTER_BOUND('',#1720,.T.);
#1284=FACE_OUTER_BOUND('',#1721,.T.);
#1285=FACE_OUTER_BOUND('',#1724,.T.);
#1286=FACE_OUTER_BOUND('',#1725,.T.);
#1287=FACE_OUTER_BOUND('',#1726,.T.);
#1288=FACE_OUTER_BOUND('',#1729,.T.);
#1289=FACE_OUTER_BOUND('',#1730,.T.);
#1290=FACE_OUTER_BOUND('',#1731,.T.);
#1291=FACE_OUTER_BOUND('',#1734,.T.);
#1292=FACE_OUTER_BOUND('',#1735,.T.);
#1293=FACE_OUTER_BOUND('',#1736,.T.);
#1294=FACE_OUTER_BOUND('',#1739,.T.);
#1295=FACE_OUTER_BOUND('',#1740,.T.);
#1296=FACE_OUTER_BOUND('',#1741,.T.);
#1297=FACE_OUTER_BOUND('',#1744,.T.);
#1298=FACE_OUTER_BOUND('',#1745,.T.);
#1299=FACE_OUTER_BOUND('',#1746,.T.);
#1300=FACE_OUTER_BOUND('',#1747,.T.);
#1301=FACE_OUTER_BOUND('',#1748,.T.);
#1302=FACE_OUTER_BOUND('',#1751,.T.);
#1303=FACE_OUTER_BOUND('',#1752,.T.);
#1304=FACE_OUTER_BOUND('',#1754,.T.);
#1305=FACE_OUTER_BOUND('',#1755,.T.);
#1306=FACE_OUTER_BOUND('',#1756,.T.);
#1307=FACE_OUTER_BOUND('',#1757,.T.);
#1308=FACE_OUTER_BOUND('',#1759,.T.);
#1309=FACE_OUTER_BOUND('',#1760,.T.);
#1310=FACE_OUTER_BOUND('',#1761,.T.);
#1311=FACE_OUTER_BOUND('',#1763,.T.);
#1312=FACE_OUTER_BOUND('',#1764,.T.);
#1313=FACE_OUTER_BOUND('',#1765,.T.);
#1314=FACE_OUTER_BOUND('',#1766,.T.);
#1315=FACE_OUTER_BOUND('',#1768,.T.);
#1316=FACE_OUTER_BOUND('',#1770,.T.);
#1317=FACE_OUTER_BOUND('',#1771,.T.);
#1318=FACE_OUTER_BOUND('',#1773,.T.);
#1319=FACE_OUTER_BOUND('',#1774,.T.);
#1320=FACE_OUTER_BOUND('',#1776,.T.);
#1321=FACE_OUTER_BOUND('',#1777,.T.);
#1322=FACE_OUTER_BOUND('',#1778,.T.);
#1323=FACE_OUTER_BOUND('',#1779,.T.);
#1324=FACE_OUTER_BOUND('',#1781,.T.);
#1325=FACE_OUTER_BOUND('',#1782,.T.);
#1326=FACE_OUTER_BOUND('',#1784,.T.);
#1327=FACE_OUTER_BOUND('',#1785,.T.);
#1328=FACE_OUTER_BOUND('',#1787,.T.);
#1329=FACE_OUTER_BOUND('',#1788,.T.);
#1330=FACE_OUTER_BOUND('',#1789,.T.);
#1331=FACE_OUTER_BOUND('',#1790,.T.);
#1332=FACE_OUTER_BOUND('',#1791,.T.);
#1333=FACE_OUTER_BOUND('',#1793,.T.);
#1334=FACE_OUTER_BOUND('',#1794,.T.);
#1335=FACE_OUTER_BOUND('',#1796,.T.);
#1336=FACE_OUTER_BOUND('',#1797,.T.);
#1337=FACE_OUTER_BOUND('',#1798,.T.);
#1338=FACE_OUTER_BOUND('',#1799,.T.);
#1339=FACE_OUTER_BOUND('',#1800,.T.);
#1340=FACE_OUTER_BOUND('',#1801,.T.);
#1341=FACE_OUTER_BOUND('',#1802,.T.);
#1342=FACE_OUTER_BOUND('',#1803,.T.);
#1343=FACE_OUTER_BOUND('',#1804,.T.);
#1344=FACE_OUTER_BOUND('',#1805,.T.);
#1345=FACE_OUTER_BOUND('',#1806,.T.);
#1346=FACE_OUTER_BOUND('',#1807,.T.);
#1347=FACE_OUTER_BOUND('',#1808,.T.);
#1348=FACE_OUTER_BOUND('',#1809,.T.);
#1349=FACE_OUTER_BOUND('',#1810,.T.);
#1350=FACE_OUTER_BOUND('',#1811,.T.);
#1351=FACE_OUTER_BOUND('',#1812,.T.);
#1352=FACE_OUTER_BOUND('',#1813,.T.);
#1353=FACE_OUTER_BOUND('',#1814,.T.);
#1354=FACE_OUTER_BOUND('',#1815,.T.);
#1355=FACE_OUTER_BOUND('',#1816,.T.);
#1356=FACE_OUTER_BOUND('',#1817,.T.);
#1357=FACE_OUTER_BOUND('',#1819,.T.);
#1358=FACE_OUTER_BOUND('',#1820,.T.);
#1359=FACE_OUTER_BOUND('',#1821,.T.);
#1360=FACE_OUTER_BOUND('',#1822,.T.);
#1361=FACE_OUTER_BOUND('',#1823,.T.);
#1362=FACE_OUTER_BOUND('',#1825,.T.);
#1363=FACE_OUTER_BOUND('',#1826,.T.);
#1364=FACE_OUTER_BOUND('',#1827,.T.);
#1365=FACE_OUTER_BOUND('',#1828,.T.);
#1366=FACE_OUTER_BOUND('',#1831,.T.);
#1367=FACE_OUTER_BOUND('',#1832,.T.);
#1368=FACE_OUTER_BOUND('',#1833,.T.);
#1369=FACE_OUTER_BOUND('',#1834,.T.);
#1370=FACE_OUTER_BOUND('',#1835,.T.);
#1371=FACE_OUTER_BOUND('',#1836,.T.);
#1372=FACE_OUTER_BOUND('',#1837,.T.);
#1373=FACE_OUTER_BOUND('',#1840,.T.);
#1374=EDGE_LOOP('',(#4459,#4460,#4461,#4462));
#1375=EDGE_LOOP('',(#4463));
#1376=EDGE_LOOP('',(#4464));
#1377=EDGE_LOOP('',(#4465,#4466,#4467,#4468));
#1378=EDGE_LOOP('',(#4469));
#1379=EDGE_LOOP('',(#4470));
#1380=EDGE_LOOP('',(#4471,#4472,#4473,#4474));
#1381=EDGE_LOOP('',(#4475));
#1382=EDGE_LOOP('',(#4476));
#1383=EDGE_LOOP('',(#4477,#4478,#4479,#4480));
#1384=EDGE_LOOP('',(#4481));
#1385=EDGE_LOOP('',(#4482));
#1386=EDGE_LOOP('',(#4483,#4484,#4485,#4486));
#1387=EDGE_LOOP('',(#4487,#4488,#4489,#4490));
#1388=EDGE_LOOP('',(#4491));
#1389=EDGE_LOOP('',(#4492));
#1390=EDGE_LOOP('',(#4493,#4494,#4495,#4496));
#1391=EDGE_LOOP('',(#4497));
#1392=EDGE_LOOP('',(#4498));
#1393=EDGE_LOOP('',(#4499,#4500,#4501,#4502));
#1394=EDGE_LOOP('',(#4503));
#1395=EDGE_LOOP('',(#4504));
#1396=EDGE_LOOP('',(#4505,#4506,#4507,#4508));
#1397=EDGE_LOOP('',(#4509,#4510,#4511,#4512));
#1398=EDGE_LOOP('',(#4513));
#1399=EDGE_LOOP('',(#4514));
#1400=EDGE_LOOP('',(#4515,#4516,#4517,#4518));
#1401=EDGE_LOOP('',(#4519));
#1402=EDGE_LOOP('',(#4520));
#1403=EDGE_LOOP('',(#4521,#4522,#4523,#4524));
#1404=EDGE_LOOP('',(#4525));
#1405=EDGE_LOOP('',(#4526));
#1406=EDGE_LOOP('',(#4527,#4528,#4529,#4530));
#1407=EDGE_LOOP('',(#4531,#4532,#4533,#4534,#4535));
#1408=EDGE_LOOP('',(#4536,#4537,#4538,#4539,#4540,#4541));
#1409=EDGE_LOOP('',(#4542,#4543,#4544,#4545,#4546,#4547,#4548,#4549));
#1410=EDGE_LOOP('',(#4550));
#1411=EDGE_LOOP('',(#4551,#4552,#4553,#4554,#4555));
#1412=EDGE_LOOP('',(#4556));
#1413=EDGE_LOOP('',(#4557));
#1414=EDGE_LOOP('',(#4558,#4559,#4560,#4561));
#1415=EDGE_LOOP('',(#4562,#4563,#4564,#4565));
#1416=EDGE_LOOP('',(#4566,#4567,#4568,#4569));
#1417=EDGE_LOOP('',(#4570,#4571,#4572,#4573));
#1418=EDGE_LOOP('',(#4574,#4575,#4576,#4577));
#1419=EDGE_LOOP('',(#4578,#4579,#4580,#4581));
#1420=EDGE_LOOP('',(#4582,#4583,#4584,#4585));
#1421=EDGE_LOOP('',(#4586,#4587,#4588,#4589));
#1422=EDGE_LOOP('',(#4590,#4591,#4592,#4593));
#1423=EDGE_LOOP('',(#4594,#4595,#4596,#4597));
#1424=EDGE_LOOP('',(#4598));
#1425=EDGE_LOOP('',(#4599,#4600,#4601,#4602));
#1426=EDGE_LOOP('',(#4603,#4604,#4605,#4606));
#1427=EDGE_LOOP('',(#4607,#4608,#4609,#4610));
#1428=EDGE_LOOP('',(#4611,#4612,#4613,#4614));
#1429=EDGE_LOOP('',(#4615,#4616,#4617,#4618));
#1430=EDGE_LOOP('',(#4619,#4620,#4621,#4622));
#1431=EDGE_LOOP('',(#4623,#4624,#4625,#4626));
#1432=EDGE_LOOP('',(#4627,#4628,#4629,#4630));
#1433=EDGE_LOOP('',(#4631,#4632,#4633,#4634));
#1434=EDGE_LOOP('',(#4635,#4636,#4637,#4638));
#1435=EDGE_LOOP('',(#4639,#4640,#4641,#4642,#4643,#4644,#4645,#4646));
#1436=EDGE_LOOP('',(#4647,#4648,#4649,#4650,#4651,#4652,#4653,#4654));
#1437=EDGE_LOOP('',(#4655,#4656,#4657,#4658));
#1438=EDGE_LOOP('',(#4659,#4660,#4661,#4662));
#1439=EDGE_LOOP('',(#4663,#4664,#4665,#4666));
#1440=EDGE_LOOP('',(#4667,#4668,#4669,#4670));
#1441=EDGE_LOOP('',(#4671,#4672,#4673,#4674));
#1442=EDGE_LOOP('',(#4675,#4676,#4677,#4678));
#1443=EDGE_LOOP('',(#4679,#4680,#4681,#4682));
#1444=EDGE_LOOP('',(#4683,#4684,#4685,#4686));
#1445=EDGE_LOOP('',(#4687,#4688,#4689,#4690));
#1446=EDGE_LOOP('',(#4691));
#1447=EDGE_LOOP('',(#4692,#4693,#4694,#4695));
#1448=EDGE_LOOP('',(#4696,#4697,#4698,#4699));
#1449=EDGE_LOOP('',(#4700,#4701,#4702,#4703));
#1450=EDGE_LOOP('',(#4704,#4705,#4706,#4707,#4708,#4709,#4710,#4711));
#1451=EDGE_LOOP('',(#4712));
#1452=EDGE_LOOP('',(#4713,#4714,#4715,#4716));
#1453=EDGE_LOOP('',(#4717));
#1454=EDGE_LOOP('',(#4718,#4719,#4720,#4721));
#1455=EDGE_LOOP('',(#4722,#4723,#4724,#4725));
#1456=EDGE_LOOP('',(#4726,#4727,#4728,#4729));
#1457=EDGE_LOOP('',(#4730,#4731,#4732,#4733));
#1458=EDGE_LOOP('',(#4734,#4735,#4736,#4737));
#1459=EDGE_LOOP('',(#4738));
#1460=EDGE_LOOP('',(#4739,#4740,#4741,#4742));
#1461=EDGE_LOOP('',(#4743,#4744,#4745,#4746));
#1462=EDGE_LOOP('',(#4747,#4748,#4749,#4750));
#1463=EDGE_LOOP('',(#4751,#4752,#4753,#4754,#4755,#4756));
#1464=EDGE_LOOP('',(#4757,#4758,#4759,#4760,#4761,#4762));
#1465=EDGE_LOOP('',(#4763,#4764,#4765,#4766,#4767));
#1466=EDGE_LOOP('',(#4768,#4769,#4770,#4771,#4772));
#1467=EDGE_LOOP('',(#4773,#4774,#4775,#4776,#4777));
#1468=EDGE_LOOP('',(#4778,#4779,#4780,#4781,#4782,#4783,#4784,#4785,#4786,
#4787,#4788));
#1469=EDGE_LOOP('',(#4789,#4790));
#1470=EDGE_LOOP('',(#4791,#4792,#4793,#4794,#4795,#4796,#4797,#4798,#4799,
#4800,#4801,#4802,#4803,#4804,#4805,#4806,#4807,#4808,#4809,#4810,#4811,
#4812,#4813,#4814,#4815,#4816,#4817,#4818,#4819,#4820,#4821,#4822,#4823,
#4824,#4825,#4826,#4827,#4828,#4829,#4830,#4831,#4832,#4833,#4834,#4835,
#4836,#4837,#4838,#4839,#4840,#4841,#4842,#4843,#4844,#4845,#4846,#4847,
#4848,#4849,#4850));
#1471=EDGE_LOOP('',(#4851));
#1472=EDGE_LOOP('',(#4852,#4853,#4854,#4855,#4856));
#1473=EDGE_LOOP('',(#4857));
#1474=EDGE_LOOP('',(#4858));
#1475=EDGE_LOOP('',(#4859,#4860,#4861,#4862,#4863));
#1476=EDGE_LOOP('',(#4864,#4865,#4866,#4867,#4868,#4869,#4870,#4871,#4872,
#4873));
#1477=EDGE_LOOP('',(#4874,#4875));
#1478=EDGE_LOOP('',(#4876,#4877,#4878));
#1479=EDGE_LOOP('',(#4879,#4880,#4881));
#1480=EDGE_LOOP('',(#4882,#4883,#4884));
#1481=EDGE_LOOP('',(#4885,#4886,#4887));
#1482=EDGE_LOOP('',(#4888,#4889,#4890));
#1483=EDGE_LOOP('',(#4891,#4892,#4893));
#1484=EDGE_LOOP('',(#4894,#4895,#4896));
#1485=EDGE_LOOP('',(#4897,#4898,#4899));
#1486=EDGE_LOOP('',(#4900,#4901,#4902));
#1487=EDGE_LOOP('',(#4903,#4904,#4905));
#1488=EDGE_LOOP('',(#4906,#4907,#4908));
#1489=EDGE_LOOP('',(#4909,#4910,#4911));
#1490=EDGE_LOOP('',(#4912,#4913,#4914));
#1491=EDGE_LOOP('',(#4915,#4916,#4917));
#1492=EDGE_LOOP('',(#4918,#4919,#4920));
#1493=EDGE_LOOP('',(#4921,#4922,#4923));
#1494=EDGE_LOOP('',(#4924,#4925,#4926));
#1495=EDGE_LOOP('',(#4927,#4928,#4929));
#1496=EDGE_LOOP('',(#4930,#4931,#4932));
#1497=EDGE_LOOP('',(#4933,#4934,#4935,#4936));
#1498=EDGE_LOOP('',(#4937,#4938,#4939,#4940));
#1499=EDGE_LOOP('',(#4941,#4942,#4943));
#1500=EDGE_LOOP('',(#4944,#4945,#4946,#4947,#4948));
#1501=EDGE_LOOP('',(#4949,#4950,#4951,#4952,#4953));
#1502=EDGE_LOOP('',(#4954,#4955,#4956,#4957,#4958));
#1503=EDGE_LOOP('',(#4959,#4960,#4961,#4962,#4963));
#1504=EDGE_LOOP('',(#4964,#4965,#4966,#4967,#4968));
#1505=EDGE_LOOP('',(#4969,#4970,#4971,#4972,#4973));
#1506=EDGE_LOOP('',(#4974,#4975,#4976,#4977,#4978));
#1507=EDGE_LOOP('',(#4979,#4980,#4981,#4982,#4983));
#1508=EDGE_LOOP('',(#4984,#4985,#4986,#4987,#4988));
#1509=EDGE_LOOP('',(#4989,#4990,#4991,#4992,#4993));
#1510=EDGE_LOOP('',(#4994,#4995,#4996,#4997,#4998,#4999));
#1511=EDGE_LOOP('',(#5000,#5001,#5002,#5003,#5004));
#1512=EDGE_LOOP('',(#5005,#5006,#5007,#5008,#5009));
#1513=EDGE_LOOP('',(#5010,#5011,#5012,#5013,#5014));
#1514=EDGE_LOOP('',(#5015,#5016,#5017,#5018,#5019));
#1515=EDGE_LOOP('',(#5020,#5021,#5022,#5023,#5024));
#1516=EDGE_LOOP('',(#5025,#5026,#5027,#5028,#5029));
#1517=EDGE_LOOP('',(#5030,#5031,#5032,#5033,#5034));
#1518=EDGE_LOOP('',(#5035,#5036,#5037,#5038,#5039));
#1519=EDGE_LOOP('',(#5040,#5041,#5042,#5043,#5044));
#1520=EDGE_LOOP('',(#5045,#5046,#5047,#5048,#5049));
#1521=EDGE_LOOP('',(#5050,#5051,#5052,#5053));
#1522=EDGE_LOOP('',(#5054,#5055,#5056,#5057,#5058,#5059,#5060,#5061,#5062,
#5063,#5064,#5065,#5066,#5067,#5068,#5069,#5070,#5071,#5072,#5073,#5074,
#5075,#5076,#5077,#5078,#5079,#5080,#5081,#5082,#5083,#5084,#5085,#5086,
#5087,#5088,#5089,#5090,#5091,#5092,#5093,#5094,#5095,#5096,#5097,#5098,
#5099,#5100,#5101,#5102,#5103,#5104,#5105,#5106,#5107,#5108,#5109,#5110,
#5111,#5112,#5113,#5114,#5115,#5116,#5117,#5118,#5119,#5120,#5121,#5122,
#5123,#5124,#5125,#5126,#5127,#5128,#5129,#5130,#5131,#5132,#5133,#5134,
#5135,#5136,#5137));
#1523=EDGE_LOOP('',(#5138,#5139,#5140,#5141,#5142));
#1524=EDGE_LOOP('',(#5143,#5144,#5145,#5146));
#1525=EDGE_LOOP('',(#5147,#5148,#5149,#5150,#5151));
#1526=EDGE_LOOP('',(#5152,#5153,#5154,#5155));
#1527=EDGE_LOOP('',(#5156,#5157,#5158,#5159,#5160));
#1528=EDGE_LOOP('',(#5161,#5162,#5163,#5164));
#1529=EDGE_LOOP('',(#5165,#5166,#5167,#5168,#5169));
#1530=EDGE_LOOP('',(#5170,#5171,#5172,#5173));
#1531=EDGE_LOOP('',(#5174,#5175,#5176,#5177,#5178));
#1532=EDGE_LOOP('',(#5179,#5180,#5181,#5182));
#1533=EDGE_LOOP('',(#5183,#5184,#5185,#5186,#5187));
#1534=EDGE_LOOP('',(#5188,#5189,#5190,#5191));
#1535=EDGE_LOOP('',(#5192,#5193,#5194,#5195,#5196));
#1536=EDGE_LOOP('',(#5197,#5198,#5199,#5200));
#1537=EDGE_LOOP('',(#5201,#5202,#5203,#5204,#5205));
#1538=EDGE_LOOP('',(#5206,#5207,#5208,#5209));
#1539=EDGE_LOOP('',(#5210,#5211,#5212,#5213,#5214,#5215));
#1540=EDGE_LOOP('',(#5216,#5217,#5218,#5219));
#1541=EDGE_LOOP('',(#5220,#5221,#5222,#5223,#5224));
#1542=EDGE_LOOP('',(#5225,#5226,#5227,#5228,#5229));
#1543=EDGE_LOOP('',(#5230,#5231,#5232,#5233,#5234));
#1544=EDGE_LOOP('',(#5235,#5236,#5237,#5238));
#1545=EDGE_LOOP('',(#5239,#5240,#5241,#5242,#5243));
#1546=EDGE_LOOP('',(#5244,#5245,#5246,#5247));
#1547=EDGE_LOOP('',(#5248,#5249,#5250,#5251,#5252));
#1548=EDGE_LOOP('',(#5253,#5254,#5255,#5256));
#1549=EDGE_LOOP('',(#5257,#5258,#5259,#5260,#5261));
#1550=EDGE_LOOP('',(#5262,#5263,#5264,#5265));
#1551=EDGE_LOOP('',(#5266,#5267,#5268,#5269,#5270));
#1552=EDGE_LOOP('',(#5271,#5272,#5273,#5274));
#1553=EDGE_LOOP('',(#5275,#5276,#5277,#5278,#5279));
#1554=EDGE_LOOP('',(#5280,#5281,#5282,#5283));
#1555=EDGE_LOOP('',(#5284,#5285,#5286,#5287,#5288));
#1556=EDGE_LOOP('',(#5289,#5290,#5291,#5292));
#1557=EDGE_LOOP('',(#5293,#5294,#5295,#5296,#5297));
#1558=EDGE_LOOP('',(#5298,#5299,#5300,#5301));
#1559=EDGE_LOOP('',(#5302,#5303,#5304,#5305,#5306));
#1560=EDGE_LOOP('',(#5307,#5308,#5309,#5310));
#1561=EDGE_LOOP('',(#5311));
#1562=EDGE_LOOP('',(#5312));
#1563=EDGE_LOOP('',(#5313,#5314,#5315,#5316,#5317,#5318));
#1564=EDGE_LOOP('',(#5319,#5320,#5321,#5322,#5323,#5324));
#1565=EDGE_LOOP('',(#5325,#5326,#5327,#5328,#5329));
#1566=EDGE_LOOP('',(#5330,#5331,#5332,#5333,#5334));
#1567=EDGE_LOOP('',(#5335,#5336,#5337,#5338,#5339));
#1568=EDGE_LOOP('',(#5340,#5341,#5342,#5343,#5344,#5345,#5346,#5347,#5348,
#5349,#5350));
#1569=EDGE_LOOP('',(#5351,#5352));
#1570=EDGE_LOOP('',(#5353,#5354,#5355,#5356,#5357,#5358,#5359,#5360,#5361,
#5362,#5363,#5364,#5365,#5366,#5367,#5368,#5369,#5370,#5371,#5372,#5373,
#5374,#5375,#5376,#5377,#5378,#5379,#5380,#5381,#5382,#5383,#5384,#5385,
#5386,#5387,#5388,#5389,#5390,#5391,#5392,#5393,#5394,#5395,#5396,#5397,
#5398,#5399,#5400,#5401,#5402,#5403,#5404,#5405,#5406,#5407,#5408,#5409,
#5410,#5411,#5412));
#1571=EDGE_LOOP('',(#5413));
#1572=EDGE_LOOP('',(#5414,#5415,#5416,#5417,#5418));
#1573=EDGE_LOOP('',(#5419));
#1574=EDGE_LOOP('',(#5420));
#1575=EDGE_LOOP('',(#5421,#5422,#5423,#5424,#5425));
#1576=EDGE_LOOP('',(#5426,#5427,#5428,#5429,#5430,#5431,#5432,#5433,#5434,
#5435));
#1577=EDGE_LOOP('',(#5436,#5437));
#1578=EDGE_LOOP('',(#5438,#5439,#5440));
#1579=EDGE_LOOP('',(#5441,#5442,#5443));
#1580=EDGE_LOOP('',(#5444,#5445,#5446));
#1581=EDGE_LOOP('',(#5447,#5448,#5449));
#1582=EDGE_LOOP('',(#5450,#5451,#5452));
#1583=EDGE_LOOP('',(#5453,#5454,#5455));
#1584=EDGE_LOOP('',(#5456,#5457,#5458));
#1585=EDGE_LOOP('',(#5459,#5460,#5461));
#1586=EDGE_LOOP('',(#5462,#5463,#5464));
#1587=EDGE_LOOP('',(#5465,#5466,#5467));
#1588=EDGE_LOOP('',(#5468,#5469,#5470));
#1589=EDGE_LOOP('',(#5471,#5472,#5473));
#1590=EDGE_LOOP('',(#5474,#5475,#5476));
#1591=EDGE_LOOP('',(#5477,#5478,#5479));
#1592=EDGE_LOOP('',(#5480,#5481,#5482));
#1593=EDGE_LOOP('',(#5483,#5484,#5485));
#1594=EDGE_LOOP('',(#5486,#5487,#5488));
#1595=EDGE_LOOP('',(#5489,#5490,#5491));
#1596=EDGE_LOOP('',(#5492,#5493,#5494));
#1597=EDGE_LOOP('',(#5495,#5496,#5497,#5498));
#1598=EDGE_LOOP('',(#5499,#5500,#5501,#5502));
#1599=EDGE_LOOP('',(#5503,#5504,#5505));
#1600=EDGE_LOOP('',(#5506,#5507,#5508,#5509,#5510));
#1601=EDGE_LOOP('',(#5511,#5512,#5513,#5514,#5515));
#1602=EDGE_LOOP('',(#5516,#5517,#5518,#5519,#5520));
#1603=EDGE_LOOP('',(#5521,#5522,#5523,#5524,#5525));
#1604=EDGE_LOOP('',(#5526,#5527,#5528,#5529,#5530));
#1605=EDGE_LOOP('',(#5531,#5532,#5533,#5534,#5535));
#1606=EDGE_LOOP('',(#5536,#5537,#5538,#5539,#5540));
#1607=EDGE_LOOP('',(#5541,#5542,#5543,#5544,#5545));
#1608=EDGE_LOOP('',(#5546,#5547,#5548,#5549,#5550));
#1609=EDGE_LOOP('',(#5551,#5552,#5553,#5554,#5555));
#1610=EDGE_LOOP('',(#5556,#5557,#5558,#5559,#5560));
#1611=EDGE_LOOP('',(#5561,#5562,#5563,#5564,#5565));
#1612=EDGE_LOOP('',(#5566,#5567,#5568,#5569,#5570));
#1613=EDGE_LOOP('',(#5571,#5572,#5573,#5574,#5575));
#1614=EDGE_LOOP('',(#5576,#5577,#5578,#5579,#5580));
#1615=EDGE_LOOP('',(#5581,#5582,#5583,#5584,#5585));
#1616=EDGE_LOOP('',(#5586,#5587,#5588,#5589,#5590));
#1617=EDGE_LOOP('',(#5591,#5592,#5593,#5594,#5595));
#1618=EDGE_LOOP('',(#5596,#5597,#5598,#5599,#5600));
#1619=EDGE_LOOP('',(#5601,#5602,#5603,#5604,#5605));
#1620=EDGE_LOOP('',(#5606,#5607,#5608,#5609,#5610));
#1621=EDGE_LOOP('',(#5611,#5612,#5613,#5614));
#1622=EDGE_LOOP('',(#5615,#5616,#5617,#5618,#5619,#5620,#5621,#5622,#5623,
#5624,#5625,#5626,#5627,#5628,#5629,#5630,#5631,#5632,#5633,#5634,#5635,
#5636,#5637,#5638,#5639,#5640,#5641,#5642,#5643,#5644,#5645,#5646,#5647,
#5648,#5649,#5650,#5651,#5652,#5653,#5654,#5655,#5656,#5657,#5658,#5659,
#5660,#5661,#5662,#5663,#5664,#5665,#5666,#5667,#5668,#5669,#5670,#5671,
#5672,#5673,#5674,#5675,#5676,#5677,#5678,#5679,#5680,#5681,#5682,#5683,
#5684,#5685,#5686,#5687,#5688,#5689,#5690,#5691,#5692,#5693,#5694,#5695,
#5696,#5697,#5698));
#1623=EDGE_LOOP('',(#5699,#5700,#5701,#5702,#5703));
#1624=EDGE_LOOP('',(#5704,#5705,#5706,#5707));
#1625=EDGE_LOOP('',(#5708,#5709,#5710,#5711,#5712));
#1626=EDGE_LOOP('',(#5713,#5714,#5715,#5716));
#1627=EDGE_LOOP('',(#5717,#5718,#5719,#5720,#5721));
#1628=EDGE_LOOP('',(#5722,#5723,#5724,#5725));
#1629=EDGE_LOOP('',(#5726,#5727,#5728,#5729,#5730));
#1630=EDGE_LOOP('',(#5731,#5732,#5733,#5734));
#1631=EDGE_LOOP('',(#5735,#5736,#5737,#5738,#5739));
#1632=EDGE_LOOP('',(#5740,#5741,#5742,#5743));
#1633=EDGE_LOOP('',(#5744,#5745,#5746,#5747,#5748));
#1634=EDGE_LOOP('',(#5749,#5750,#5751,#5752));
#1635=EDGE_LOOP('',(#5753,#5754,#5755,#5756,#5757));
#1636=EDGE_LOOP('',(#5758,#5759,#5760,#5761));
#1637=EDGE_LOOP('',(#5762,#5763,#5764,#5765,#5766));
#1638=EDGE_LOOP('',(#5767,#5768,#5769,#5770));
#1639=EDGE_LOOP('',(#5771,#5772,#5773,#5774,#5775));
#1640=EDGE_LOOP('',(#5776,#5777,#5778,#5779,#5780));
#1641=EDGE_LOOP('',(#5781,#5782,#5783,#5784,#5785));
#1642=EDGE_LOOP('',(#5786,#5787,#5788,#5789));
#1643=EDGE_LOOP('',(#5790,#5791,#5792,#5793,#5794));
#1644=EDGE_LOOP('',(#5795,#5796,#5797,#5798));
#1645=EDGE_LOOP('',(#5799,#5800,#5801,#5802,#5803));
#1646=EDGE_LOOP('',(#5804,#5805,#5806,#5807));
#1647=EDGE_LOOP('',(#5808,#5809,#5810,#5811,#5812));
#1648=EDGE_LOOP('',(#5813,#5814,#5815,#5816));
#1649=EDGE_LOOP('',(#5817,#5818,#5819,#5820,#5821));
#1650=EDGE_LOOP('',(#5822,#5823,#5824,#5825));
#1651=EDGE_LOOP('',(#5826,#5827,#5828,#5829,#5830));
#1652=EDGE_LOOP('',(#5831,#5832,#5833,#5834));
#1653=EDGE_LOOP('',(#5835,#5836,#5837,#5838,#5839));
#1654=EDGE_LOOP('',(#5840,#5841,#5842,#5843));
#1655=EDGE_LOOP('',(#5844,#5845,#5846,#5847,#5848));
#1656=EDGE_LOOP('',(#5849,#5850,#5851,#5852));
#1657=EDGE_LOOP('',(#5853,#5854,#5855,#5856,#5857));
#1658=EDGE_LOOP('',(#5858,#5859,#5860,#5861));
#1659=EDGE_LOOP('',(#5862,#5863,#5864,#5865,#5866));
#1660=EDGE_LOOP('',(#5867,#5868,#5869,#5870));
#1661=EDGE_LOOP('',(#5871));
#1662=EDGE_LOOP('',(#5872));
#1663=EDGE_LOOP('',(#5873,#5874,#5875));
#1664=EDGE_LOOP('',(#5876,#5877,#5878));
#1665=EDGE_LOOP('',(#5879,#5880,#5881,#5882));
#1666=EDGE_LOOP('',(#5883,#5884));
#1667=EDGE_LOOP('',(#5885,#5886,#5887,#5888));
#1668=EDGE_LOOP('',(#5889,#5890));
#1669=EDGE_LOOP('',(#5891,#5892,#5893));
#1670=EDGE_LOOP('',(#5894,#5895,#5896,#5897));
#1671=EDGE_LOOP('',(#5898,#5899,#5900,#5901));
#1672=EDGE_LOOP('',(#5902,#5903,#5904));
#1673=EDGE_LOOP('',(#5905));
#1674=EDGE_LOOP('',(#5906));
#1675=EDGE_LOOP('',(#5907,#5908,#5909,#5910));
#1676=EDGE_LOOP('',(#5911,#5912,#5913,#5914,#5915,#5916,#5917,#5918,#5919,
#5920,#5921,#5922));
#1677=EDGE_LOOP('',(#5923,#5924,#5925,#5926));
#1678=EDGE_LOOP('',(#5927,#5928,#5929,#5930));
#1679=EDGE_LOOP('',(#5931));
#1680=EDGE_LOOP('',(#5932));
#1681=EDGE_LOOP('',(#5933,#5934,#5935));
#1682=EDGE_LOOP('',(#5936,#5937,#5938));
#1683=EDGE_LOOP('',(#5939,#5940,#5941,#5942));
#1684=EDGE_LOOP('',(#5943,#5944));
#1685=EDGE_LOOP('',(#5945,#5946,#5947,#5948));
#1686=EDGE_LOOP('',(#5949,#5950));
#1687=EDGE_LOOP('',(#5951,#5952,#5953));
#1688=EDGE_LOOP('',(#5954,#5955,#5956,#5957));
#1689=EDGE_LOOP('',(#5958,#5959,#5960,#5961));
#1690=EDGE_LOOP('',(#5962,#5963,#5964));
#1691=EDGE_LOOP('',(#5965));
#1692=EDGE_LOOP('',(#5966));
#1693=EDGE_LOOP('',(#5967,#5968,#5969,#5970));
#1694=EDGE_LOOP('',(#5971,#5972,#5973,#5974,#5975,#5976,#5977,#5978,#5979,
#5980,#5981,#5982));
#1695=EDGE_LOOP('',(#5983,#5984,#5985,#5986));
#1696=EDGE_LOOP('',(#5987,#5988,#5989,#5990));
#1697=EDGE_LOOP('',(#5991));
#1698=EDGE_LOOP('',(#5992));
#1699=EDGE_LOOP('',(#5993,#5994));
#1700=EDGE_LOOP('',(#5995,#5996,#5997,#5998));
#1701=EDGE_LOOP('',(#5999,#6000,#6001,#6002));
#1702=EDGE_LOOP('',(#6003,#6004,#6005,#6006,#6007,#6008,#6009,#6010,#6011,
#6012,#6013,#6014,#6015,#6016,#6017,#6018,#6019,#6020,#6021,#6022,#6023,
#6024,#6025,#6026));
#1703=EDGE_LOOP('',(#6027,#6028,#6029,#6030));
#1704=EDGE_LOOP('',(#6031,#6032,#6033,#6034,#6035,#6036,#6037,#6038,#6039,
#6040,#6041,#6042,#6043,#6044,#6045,#6046,#6047,#6048,#6049,#6050,#6051,
#6052,#6053,#6054));
#1705=EDGE_LOOP('',(#6055,#6056,#6057,#6058));
#1706=EDGE_LOOP('',(#6059,#6060));
#1707=EDGE_LOOP('',(#6061,#6062,#6063,#6064));
#1708=EDGE_LOOP('',(#6065,#6066,#6067,#6068));
#1709=EDGE_LOOP('',(#6069,#6070,#6071,#6072));
#1710=EDGE_LOOP('',(#6073,#6074,#6075,#6076));
#1711=EDGE_LOOP('',(#6077,#6078));
#1712=EDGE_LOOP('',(#6079,#6080,#6081,#6082));
#1713=EDGE_LOOP('',(#6083,#6084,#6085,#6086));
#1714=EDGE_LOOP('',(#6087,#6088,#6089,#6090));
#1715=EDGE_LOOP('',(#6091,#6092,#6093,#6094));
#1716=EDGE_LOOP('',(#6095,#6096));
#1717=EDGE_LOOP('',(#6097,#6098,#6099,#6100));
#1718=EDGE_LOOP('',(#6101,#6102,#6103,#6104));
#1719=EDGE_LOOP('',(#6105,#6106,#6107,#6108));
#1720=EDGE_LOOP('',(#6109,#6110,#6111,#6112));
#1721=EDGE_LOOP('',(#6113,#6114));
#1722=EDGE_LOOP('',(#6115,#6116,#6117,#6118,#6119,#6120));
#1723=EDGE_LOOP('',(#6121,#6122,#6123,#6124,#6125,#6126));
#1724=EDGE_LOOP('',(#6127,#6128,#6129,#6130));
#1725=EDGE_LOOP('',(#6131,#6132,#6133,#6134));
#1726=EDGE_LOOP('',(#6135,#6136));
#1727=EDGE_LOOP('',(#6137,#6138,#6139,#6140));
#1728=EDGE_LOOP('',(#6141,#6142,#6143,#6144));
#1729=EDGE_LOOP('',(#6145,#6146,#6147,#6148));
#1730=EDGE_LOOP('',(#6149,#6150,#6151,#6152));
#1731=EDGE_LOOP('',(#6153,#6154));
#1732=EDGE_LOOP('',(#6155,#6156,#6157,#6158));
#1733=EDGE_LOOP('',(#6159,#6160,#6161,#6162));
#1734=EDGE_LOOP('',(#6163,#6164,#6165,#6166));
#1735=EDGE_LOOP('',(#6167,#6168,#6169,#6170));
#1736=EDGE_LOOP('',(#6171,#6172));
#1737=EDGE_LOOP('',(#6173,#6174,#6175,#6176));
#1738=EDGE_LOOP('',(#6177,#6178,#6179,#6180));
#1739=EDGE_LOOP('',(#6181,#6182,#6183,#6184));
#1740=EDGE_LOOP('',(#6185,#6186,#6187,#6188));
#1741=EDGE_LOOP('',(#6189,#6190));
#1742=EDGE_LOOP('',(#6191,#6192,#6193,#6194));
#1743=EDGE_LOOP('',(#6195,#6196,#6197,#6198));
#1744=EDGE_LOOP('',(#6199,#6200,#6201,#6202,#6203,#6204,#6205,#6206,#6207,
#6208,#6209,#6210,#6211,#6212,#6213,#6214,#6215,#6216,#6217,#6218,#6219,
#6220,#6221,#6222));
#1745=EDGE_LOOP('',(#6223,#6224,#6225,#6226));
#1746=EDGE_LOOP('',(#6227,#6228,#6229,#6230,#6231,#6232,#6233,#6234,#6235,
#6236,#6237,#6238,#6239,#6240,#6241,#6242,#6243,#6244,#6245,#6246,#6247,
#6248,#6249,#6250));
#1747=EDGE_LOOP('',(#6251,#6252,#6253,#6254));
#1748=EDGE_LOOP('',(#6255,#6256));
#1749=EDGE_LOOP('',(#6257,#6258,#6259,#6260));
#1750=EDGE_LOOP('',(#6261,#6262,#6263,#6264));
#1751=EDGE_LOOP('',(#6265,#6266,#6267,#6268));
#1752=EDGE_LOOP('',(#6269));
#1753=EDGE_LOOP('',(#6270));
#1754=EDGE_LOOP('',(#6271,#6272,#6273,#6274));
#1755=EDGE_LOOP('',(#6275,#6276,#6277,#6278));
#1756=EDGE_LOOP('',(#6279,#6280,#6281,#6282));
#1757=EDGE_LOOP('',(#6283));
#1758=EDGE_LOOP('',(#6284));
#1759=EDGE_LOOP('',(#6285,#6286,#6287,#6288));
#1760=EDGE_LOOP('',(#6289,#6290,#6291,#6292));
#1761=EDGE_LOOP('',(#6293));
#1762=EDGE_LOOP('',(#6294));
#1763=EDGE_LOOP('',(#6295,#6296,#6297,#6298));
#1764=EDGE_LOOP('',(#6299,#6300,#6301,#6302));
#1765=EDGE_LOOP('',(#6303,#6304,#6305,#6306));
#1766=EDGE_LOOP('',(#6307));
#1767=EDGE_LOOP('',(#6308));
#1768=EDGE_LOOP('',(#6309));
#1769=EDGE_LOOP('',(#6310));
#1770=EDGE_LOOP('',(#6311,#6312,#6313,#6314));
#1771=EDGE_LOOP('',(#6315));
#1772=EDGE_LOOP('',(#6316));
#1773=EDGE_LOOP('',(#6317,#6318,#6319,#6320));
#1774=EDGE_LOOP('',(#6321));
#1775=EDGE_LOOP('',(#6322));
#1776=EDGE_LOOP('',(#6323,#6324,#6325,#6326));
#1777=EDGE_LOOP('',(#6327,#6328,#6329,#6330));
#1778=EDGE_LOOP('',(#6331,#6332,#6333,#6334));
#1779=EDGE_LOOP('',(#6335));
#1780=EDGE_LOOP('',(#6336));
#1781=EDGE_LOOP('',(#6337,#6338,#6339,#6340));
#1782=EDGE_LOOP('',(#6341));
#1783=EDGE_LOOP('',(#6342));
#1784=EDGE_LOOP('',(#6343,#6344,#6345,#6346));
#1785=EDGE_LOOP('',(#6347));
#1786=EDGE_LOOP('',(#6348));
#1787=EDGE_LOOP('',(#6349,#6350,#6351,#6352));
#1788=EDGE_LOOP('',(#6353,#6354,#6355,#6356));
#1789=EDGE_LOOP('',(#6357,#6358,#6359,#6360));
#1790=EDGE_LOOP('',(#6361,#6362,#6363,#6364));
#1791=EDGE_LOOP('',(#6365));
#1792=EDGE_LOOP('',(#6366));
#1793=EDGE_LOOP('',(#6367,#6368,#6369,#6370));
#1794=EDGE_LOOP('',(#6371));
#1795=EDGE_LOOP('',(#6372));
#1796=EDGE_LOOP('',(#6373,#6374,#6375,#6376));
#1797=EDGE_LOOP('',(#6377,#6378,#6379,#6380));
#1798=EDGE_LOOP('',(#6381,#6382,#6383,#6384));
#1799=EDGE_LOOP('',(#6385,#6386,#6387,#6388));
#1800=EDGE_LOOP('',(#6389,#6390,#6391,#6392));
#1801=EDGE_LOOP('',(#6393,#6394,#6395,#6396));
#1802=EDGE_LOOP('',(#6397,#6398,#6399,#6400));
#1803=EDGE_LOOP('',(#6401,#6402,#6403,#6404));
#1804=EDGE_LOOP('',(#6405,#6406,#6407,#6408));
#1805=EDGE_LOOP('',(#6409,#6410,#6411,#6412,#6413));
#1806=EDGE_LOOP('',(#6414,#6415,#6416,#6417,#6418,#6419,#6420,#6421,#6422,
#6423,#6424,#6425,#6426));
#1807=EDGE_LOOP('',(#6427,#6428,#6429,#6430,#6431));
#1808=EDGE_LOOP('',(#6432,#6433,#6434,#6435));
#1809=EDGE_LOOP('',(#6436,#6437,#6438,#6439,#6440,#6441,#6442,#6443,#6444,
#6445,#6446,#6447,#6448));
#1810=EDGE_LOOP('',(#6449,#6450,#6451));
#1811=EDGE_LOOP('',(#6452,#6453,#6454,#6455));
#1812=EDGE_LOOP('',(#6456,#6457,#6458,#6459));
#1813=EDGE_LOOP('',(#6460,#6461,#6462,#6463));
#1814=EDGE_LOOP('',(#6464,#6465,#6466,#6467));
#1815=EDGE_LOOP('',(#6468,#6469,#6470,#6471));
#1816=EDGE_LOOP('',(#6472,#6473,#6474,#6475));
#1817=EDGE_LOOP('',(#6476,#6477,#6478,#6479,#6480,#6481));
#1818=EDGE_LOOP('',(#6482));
#1819=EDGE_LOOP('',(#6483));
#1820=EDGE_LOOP('',(#6484,#6485,#6486,#6487,#6488,#6489));
#1821=EDGE_LOOP('',(#6490,#6491,#6492,#6493));
#1822=EDGE_LOOP('',(#6494,#6495,#6496,#6497,#6498,#6499));
#1823=EDGE_LOOP('',(#6500));
#1824=EDGE_LOOP('',(#6501,#6502,#6503,#6504,#6505,#6506));
#1825=EDGE_LOOP('',(#6507,#6508,#6509,#6510));
#1826=EDGE_LOOP('',(#6511,#6512,#6513,#6514));
#1827=EDGE_LOOP('',(#6515,#6516,#6517,#6518));
#1828=EDGE_LOOP('',(#6519,#6520,#6521,#6522,#6523,#6524,#6525,#6526));
#1829=EDGE_LOOP('',(#6527));
#1830=EDGE_LOOP('',(#6528));
#1831=EDGE_LOOP('',(#6529,#6530,#6531,#6532));
#1832=EDGE_LOOP('',(#6533,#6534,#6535,#6536));
#1833=EDGE_LOOP('',(#6537,#6538,#6539,#6540));
#1834=EDGE_LOOP('',(#6541,#6542,#6543,#6544));
#1835=EDGE_LOOP('',(#6545,#6546,#6547,#6548));
#1836=EDGE_LOOP('',(#6549,#6550,#6551,#6552));
#1837=EDGE_LOOP('',(#6553,#6554,#6555,#6556,#6557,#6558,#6559,#6560));
#1838=EDGE_LOOP('',(#6561));
#1839=EDGE_LOOP('',(#6562));
#1840=EDGE_LOOP('',(#6563,#6564,#6565,#6566));
#1841=LINE('',#9466,#2100);
#1842=LINE('',#9473,#2101);
#1843=LINE('',#9480,#2102);
#1844=LINE('',#9487,#2103);
#1845=LINE('',#9494,#2104);
#1846=LINE('',#9500,#2105);
#1847=LINE('',#9507,#2106);
#1848=LINE('',#9514,#2107);
#1849=LINE('',#9521,#2108);
#1850=LINE('',#9527,#2109);
#1851=LINE('',#9534,#2110);
#1852=LINE('',#9541,#2111);
#1853=LINE('',#9548,#2112);
#1854=LINE('',#9560,#2113);
#1855=LINE('',#9567,#2114);
#1856=LINE('',#9571,#2115);
#1857=LINE('',#9575,#2116);
#1858=LINE('',#9579,#2117);
#1859=LINE('',#9583,#2118);
#1860=LINE('',#9588,#2119);
#1861=LINE('',#9590,#2120);
#1862=LINE('',#9591,#2121);
#1863=LINE('',#9595,#2122);
#1864=LINE('',#9598,#2123);
#1865=LINE('',#9599,#2124);
#1866=LINE('',#9603,#2125);
#1867=LINE('',#9606,#2126);
#1868=LINE('',#9607,#2127);
#1869=LINE('',#9611,#2128);
#1870=LINE('',#9614,#2129);
#1871=LINE('',#9615,#2130);
#1872=LINE('',#9620,#2131);
#1873=LINE('',#9623,#2132);
#1874=LINE('',#9626,#2133);
#1875=LINE('',#9627,#2134);
#1876=LINE('',#9630,#2135);
#1877=LINE('',#9634,#2136);
#1878=LINE('',#9635,#2137);
#1879=LINE('',#9638,#2138);
#1880=LINE('',#9640,#2139);
#1881=LINE('',#9645,#2140);
#1882=LINE('',#9646,#2141);
#1883=LINE('',#9647,#2142);
#1884=LINE('',#9651,#2143);
#1885=LINE('',#9656,#2144);
#1886=LINE('',#9658,#2145);
#1887=LINE('',#9659,#2146);
#1888=LINE('',#9662,#2147);
#1889=LINE('',#9667,#2148);
#1890=LINE('',#9668,#2149);
#1891=LINE('',#9671,#2150);
#1892=LINE('',#9674,#2151);
#1893=LINE('',#9680,#2152);
#1894=LINE('',#9684,#2153);
#1895=LINE('',#9688,#2154);
#1896=LINE('',#9691,#2155);
#1897=LINE('',#9694,#2156);
#1898=LINE('',#9697,#2157);
#1899=LINE('',#9700,#2158);
#1900=LINE('',#9701,#2159);
#1901=LINE('',#9704,#2160);
#1902=LINE('',#9708,#2161);
#1903=LINE('',#9709,#2162);
#1904=LINE('',#9712,#2163);
#1905=LINE('',#9716,#2164);
#1906=LINE('',#9717,#2165);
#1907=LINE('',#9720,#2166);
#1908=LINE('',#9723,#2167);
#1909=LINE('',#9726,#2168);
#1910=LINE('',#9728,#2169);
#1911=LINE('',#9729,#2170);
#1912=LINE('',#9732,#2171);
#1913=LINE('',#9736,#2172);
#1914=LINE('',#9737,#2173);
#1915=LINE('',#9740,#2174);
#1916=LINE('',#9744,#2175);
#1917=LINE('',#9748,#2176);
#1918=LINE('',#9751,#2177);
#1919=LINE('',#9753,#2178);
#1920=LINE('',#9755,#2179);
#1921=LINE('',#9758,#2180);
#1922=LINE('',#9759,#2181);
#1923=LINE('',#9761,#2182);
#1924=LINE('',#9768,#2183);
#1925=LINE('',#9826,#2184);
#1926=LINE('',#9830,#2185);
#1927=LINE('',#9893,#2186);
#1928=LINE('',#9916,#2187);
#1929=LINE('',#9958,#2188);
#1930=LINE('',#9967,#2189);
#1931=LINE('',#9968,#2190);
#1932=LINE('',#11449,#2191);
#1933=LINE('',#11456,#2192);
#1934=LINE('',#11461,#2193);
#1935=LINE('',#11463,#2194);
#1936=LINE('',#12058,#2195);
#1937=LINE('',#12062,#2196);
#1938=LINE('',#12119,#2197);
#1939=LINE('',#12179,#2198);
#1940=LINE('',#12239,#2199);
#1941=LINE('',#12299,#2200);
#1942=LINE('',#12359,#2201);
#1943=LINE('',#12419,#2202);
#1944=LINE('',#12479,#2203);
#1945=LINE('',#12539,#2204);
#1946=LINE('',#12599,#2205);
#1947=LINE('',#12659,#2206);
#1948=LINE('',#12719,#2207);
#1949=LINE('',#12755,#2208);
#1950=LINE('',#12815,#2209);
#1951=LINE('',#12875,#2210);
#1952=LINE('',#12935,#2211);
#1953=LINE('',#12995,#2212);
#1954=LINE('',#13055,#2213);
#1955=LINE('',#13115,#2214);
#1956=LINE('',#13175,#2215);
#1957=LINE('',#13235,#2216);
#1958=LINE('',#13432,#2217);
#1959=LINE('',#15887,#2218);
#1960=LINE('',#15891,#2219);
#1961=LINE('',#15954,#2220);
#1962=LINE('',#15977,#2221);
#1963=LINE('',#16019,#2222);
#1964=LINE('',#16028,#2223);
#1965=LINE('',#16029,#2224);
#1966=LINE('',#17513,#2225);
#1967=LINE('',#17520,#2226);
#1968=LINE('',#17525,#2227);
#1969=LINE('',#17527,#2228);
#1970=LINE('',#18084,#2229);
#1971=LINE('',#18088,#2230);
#1972=LINE('',#18143,#2231);
#1973=LINE('',#18203,#2232);
#1974=LINE('',#18263,#2233);
#1975=LINE('',#18323,#2234);
#1976=LINE('',#18383,#2235);
#1977=LINE('',#18443,#2236);
#1978=LINE('',#18503,#2237);
#1979=LINE('',#18563,#2238);
#1980=LINE('',#18623,#2239);
#1981=LINE('',#18683,#2240);
#1982=LINE('',#18743,#2241);
#1983=LINE('',#18803,#2242);
#1984=LINE('',#18863,#2243);
#1985=LINE('',#18923,#2244);
#1986=LINE('',#18983,#2245);
#1987=LINE('',#19043,#2246);
#1988=LINE('',#19103,#2247);
#1989=LINE('',#19163,#2248);
#1990=LINE('',#19223,#2249);
#1991=LINE('',#19283,#2250);
#1992=LINE('',#19402,#2251);
#1993=LINE('',#20982,#2252);
#1994=LINE('',#20989,#2253);
#1995=LINE('',#20992,#2254);
#1996=LINE('',#20993,#2255);
#1997=LINE('',#20998,#2256);
#1998=LINE('',#21001,#2257);
#1999=LINE('',#21003,#2258);
#2000=LINE('',#21004,#2259);
#2001=LINE('',#21010,#2260);
#2002=LINE('',#21014,#2261);
#2003=LINE('',#21020,#2262);
#2004=LINE('',#21024,#2263);
#2005=LINE('',#21031,#2264);
#2006=LINE('',#21035,#2265);
#2007=LINE('',#21036,#2266);
#2008=LINE('',#21040,#2267);
#2009=LINE('',#21048,#2268);
#2010=LINE('',#21055,#2269);
#2011=LINE('',#21058,#2270);
#2012=LINE('',#21059,#2271);
#2013=LINE('',#21064,#2272);
#2014=LINE('',#21067,#2273);
#2015=LINE('',#21069,#2274);
#2016=LINE('',#21070,#2275);
#2017=LINE('',#21076,#2276);
#2018=LINE('',#21080,#2277);
#2019=LINE('',#21086,#2278);
#2020=LINE('',#21090,#2279);
#2021=LINE('',#21097,#2280);
#2022=LINE('',#21101,#2281);
#2023=LINE('',#21102,#2282);
#2024=LINE('',#21106,#2283);
#2025=LINE('',#21191,#2284);
#2026=LINE('',#21326,#2285);
#2027=LINE('',#21911,#2286);
#2028=LINE('',#21928,#2287);
#2029=LINE('',#21982,#2288);
#2030=LINE('',#21986,#2289);
#2031=LINE('',#21990,#2290);
#2032=LINE('',#21995,#2291);
#2033=LINE('',#22002,#2292);
#2034=LINE('',#22006,#2293);
#2035=LINE('',#22010,#2294);
#2036=LINE('',#22022,#2295);
#2037=LINE('',#22028,#2296);
#2038=LINE('',#22036,#2297);
#2039=LINE('',#22040,#2298);
#2040=LINE('',#22044,#2299);
#2041=LINE('',#22050,#2300);
#2042=LINE('',#22058,#2301);
#2043=LINE('',#22064,#2302);
#2044=LINE('',#22068,#2303);
#2045=LINE('',#22071,#2304);
#2046=LINE('',#22077,#2305);
#2047=LINE('',#22084,#2306);
#2048=LINE('',#22091,#2307);
#2049=LINE('',#22115,#2308);
#2050=LINE('',#22163,#2309);
#2051=LINE('',#22217,#2310);
#2052=LINE('',#22265,#2311);
#2053=LINE('',#22316,#2312);
#2054=LINE('',#22342,#2313);
#2055=LINE('',#22366,#2314);
#2056=LINE('',#22391,#2315);
#2057=LINE('',#23099,#2316);
#2058=LINE('',#23104,#2317);
#2059=LINE('',#23106,#2318);
#2060=LINE('',#23108,#2319);
#2061=LINE('',#23109,#2320);
#2062=LINE('',#23112,#2321);
#2063=LINE('',#23114,#2322);
#2064=LINE('',#23115,#2323);
#2065=LINE('',#23118,#2324);
#2066=LINE('',#23120,#2325);
#2067=LINE('',#23121,#2326);
#2068=LINE('',#23124,#2327);
#2069=LINE('',#23126,#2328);
#2070=LINE('',#23127,#2329);
#2071=LINE('',#23130,#2330);
#2072=LINE('',#23132,#2331);
#2073=LINE('',#23133,#2332);
#2074=LINE('',#23135,#2333);
#2075=LINE('',#23136,#2334);
#2076=LINE('',#23142,#2335);
#2077=LINE('',#23148,#2336);
#2078=LINE('',#23155,#2337);
#2079=LINE('',#23161,#2338);
#2080=LINE('',#23166,#2339);
#2081=LINE('',#23170,#2340);
#2082=LINE('',#23174,#2341);
#2083=LINE('',#23176,#2342);
#2084=LINE('',#23178,#2343);
#2085=LINE('',#23182,#2344);
#2086=LINE('',#23184,#2345);
#2087=LINE('',#23185,#2346);
#2088=LINE('',#23188,#2347);
#2089=LINE('',#23190,#2348);
#2090=LINE('',#23191,#2349);
#2091=LINE('',#23194,#2350);
#2092=LINE('',#23195,#2351);
#2093=LINE('',#23197,#2352);
#2094=LINE('',#23200,#2353);
#2095=LINE('',#23201,#2354);
#2096=LINE('',#23204,#2355);
#2097=LINE('',#23206,#2356);
#2098=LINE('',#23207,#2357);
#2099=LINE('',#23209,#2358);
#2100=VECTOR('',#7839,14.);
#2101=VECTOR('',#7848,14.7);
#2102=VECTOR('',#7857,14.);
#2103=VECTOR('',#7866,12.);
#2104=VECTOR('',#7875,14.);
#2105=VECTOR('',#7882,14.);
#2106=VECTOR('',#7891,14.7);
#2107=VECTOR('',#7900,14.);
#2108=VECTOR('',#7909,12.);
#2109=VECTOR('',#7916,12.);
#2110=VECTOR('',#7925,14.);
#2111=VECTOR('',#7934,14.7);
#2112=VECTOR('',#7943,14.);
#2113=VECTOR('',#7958,20.);
#2114=VECTOR('',#7965,10.);
#2115=VECTOR('',#7968,10.);
#2116=VECTOR('',#7971,10.);
#2117=VECTOR('',#7974,10.);
#2118=VECTOR('',#7979,19.5);
#2119=VECTOR('',#7986,10.);
#2120=VECTOR('',#7987,10.);
#2121=VECTOR('',#7988,10.);
#2122=VECTOR('',#7993,10.);
#2123=VECTOR('',#7996,10.);
#2124=VECTOR('',#7997,10.);
#2125=VECTOR('',#8002,10.);
#2126=VECTOR('',#8005,10.);
#2127=VECTOR('',#8006,10.);
#2128=VECTOR('',#8011,10.);
#2129=VECTOR('',#8014,10.);
#2130=VECTOR('',#8015,10.);
#2131=VECTOR('',#8022,10.);
#2132=VECTOR('',#8025,10.);
#2133=VECTOR('',#8028,10.);
#2134=VECTOR('',#8029,10.);
#2135=VECTOR('',#8032,10.);
#2136=VECTOR('',#8037,10.);
#2137=VECTOR('',#8038,10.);
#2138=VECTOR('',#8041,10.);
#2139=VECTOR('',#8042,10.);
#2140=VECTOR('',#8047,10.);
#2141=VECTOR('',#8048,10.);
#2142=VECTOR('',#8049,10.);
#2143=VECTOR('',#8052,10.);
#2144=VECTOR('',#8059,10.);
#2145=VECTOR('',#8060,10.);
#2146=VECTOR('',#8061,10.);
#2147=VECTOR('',#8064,10.);
#2148=VECTOR('',#8071,10.);
#2149=VECTOR('',#8072,10.);
#2150=VECTOR('',#8075,10.);
#2151=VECTOR('',#8080,10.);
#2152=VECTOR('',#8085,10.);
#2153=VECTOR('',#8088,10.);
#2154=VECTOR('',#8091,10.);
#2155=VECTOR('',#8094,10.);
#2156=VECTOR('',#8097,10.);
#2157=VECTOR('',#8100,10.);
#2158=VECTOR('',#8103,10.);
#2159=VECTOR('',#8104,10.);
#2160=VECTOR('',#8107,10.);
#2161=VECTOR('',#8112,10.);
#2162=VECTOR('',#8113,10.);
#2163=VECTOR('',#8116,10.);
#2164=VECTOR('',#8121,10.);
#2165=VECTOR('',#8122,10.);
#2166=VECTOR('',#8125,10.);
#2167=VECTOR('',#8130,10.);
#2168=VECTOR('',#8133,10.);
#2169=VECTOR('',#8134,10.);
#2170=VECTOR('',#8135,10.);
#2171=VECTOR('',#8138,10.);
#2172=VECTOR('',#8143,10.);
#2173=VECTOR('',#8144,10.);
#2174=VECTOR('',#8147,10.);
#2175=VECTOR('',#8152,10.);
#2176=VECTOR('',#8155,10.);
#2177=VECTOR('',#8160,10.);
#2178=VECTOR('',#8163,10.);
#2179=VECTOR('',#8166,10.);
#2180=VECTOR('',#8171,10.);
#2181=VECTOR('',#8172,10.);
#2182=VECTOR('',#8175,10.);
#2183=VECTOR('',#8184,12.1473403730037);
#2184=VECTOR('',#8189,2.175);
#2185=VECTOR('',#8194,2.05);
#2186=VECTOR('',#8197,2.175);
#2187=VECTOR('',#8202,2.05);
#2188=VECTOR('',#8207,6.275);
#2189=VECTOR('',#8218,6.025);
#2190=VECTOR('',#8219,6.025);
#2191=VECTOR('',#8262,6.275);
#2192=VECTOR('',#8271,9.75);
#2193=VECTOR('',#8278,10.);
#2194=VECTOR('',#8279,10.);
#2195=VECTOR('',#8362,14.5);
#2196=VECTOR('',#8367,10.5);
#2197=VECTOR('',#8374,8.74592262443523);
#2198=VECTOR('',#8375,8.74592262443523);
#2199=VECTOR('',#8376,8.74592262443523);
#2200=VECTOR('',#8377,8.74592262443523);
#2201=VECTOR('',#8378,8.74592262443523);
#2202=VECTOR('',#8379,8.74592262443523);
#2203=VECTOR('',#8380,8.74592262443523);
#2204=VECTOR('',#8381,8.74592262443523);
#2205=VECTOR('',#8382,8.74592262443523);
#2206=VECTOR('',#8383,8.74592262443523);
#2207=VECTOR('',#8384,8.74592262443523);
#2208=VECTOR('',#8385,8.74592262443523);
#2209=VECTOR('',#8386,8.74592262443523);
#2210=VECTOR('',#8387,8.74592262443523);
#2211=VECTOR('',#8388,8.74592262443523);
#2212=VECTOR('',#8389,8.74592262443523);
#2213=VECTOR('',#8390,8.74592262443523);
#2214=VECTOR('',#8391,8.74592262443523);
#2215=VECTOR('',#8392,8.74592262443523);
#2216=VECTOR('',#8393,8.74592262443523);
#2217=VECTOR('',#8400,12.1473403730037);
#2218=VECTOR('',#8485,2.175);
#2219=VECTOR('',#8490,2.05);
#2220=VECTOR('',#8493,2.175);
#2221=VECTOR('',#8498,2.05);
#2222=VECTOR('',#8503,6.275);
#2223=VECTOR('',#8514,6.025);
#2224=VECTOR('',#8515,6.025);
#2225=VECTOR('',#8560,6.275);
#2226=VECTOR('',#8569,9.75);
#2227=VECTOR('',#8576,10.);
#2228=VECTOR('',#8577,10.);
#2229=VECTOR('',#8660,14.5);
#2230=VECTOR('',#8665,10.5);
#2231=VECTOR('',#8672,8.74592262443523);
#2232=VECTOR('',#8673,8.74592262443523);
#2233=VECTOR('',#8674,8.74592262443523);
#2234=VECTOR('',#8675,8.74592262443523);
#2235=VECTOR('',#8676,8.74592262443523);
#2236=VECTOR('',#8677,8.74592262443523);
#2237=VECTOR('',#8678,8.74592262443523);
#2238=VECTOR('',#8679,8.74592262443523);
#2239=VECTOR('',#8680,8.74592262443523);
#2240=VECTOR('',#8681,8.74592262443523);
#2241=VECTOR('',#8682,8.74592262443523);
#2242=VECTOR('',#8683,8.74592262443523);
#2243=VECTOR('',#8684,8.74592262443523);
#2244=VECTOR('',#8685,8.74592262443523);
#2245=VECTOR('',#8686,8.74592262443523);
#2246=VECTOR('',#8687,8.74592262443523);
#2247=VECTOR('',#8688,8.74592262443523);
#2248=VECTOR('',#8689,8.74592262443523);
#2249=VECTOR('',#8690,8.74592262443523);
#2250=VECTOR('',#8691,8.74592262443523);
#2251=VECTOR('',#8698,12.1473403730037);
#2252=VECTOR('',#8785,10.);
#2253=VECTOR('',#8792,10.);
#2254=VECTOR('',#8797,10.);
#2255=VECTOR('',#8798,10.);
#2256=VECTOR('',#8803,10.);
#2257=VECTOR('',#8806,10.);
#2258=VECTOR('',#8807,10.);
#2259=VECTOR('',#8808,10.);
#2260=VECTOR('',#8815,0.625);
#2261=VECTOR('',#8820,1.25);
#2262=VECTOR('',#8827,1.25);
#2263=VECTOR('',#8832,1.25);
#2264=VECTOR('',#8841,5.6);
#2265=VECTOR('',#8846,6.);
#2266=VECTOR('',#8847,6.);
#2267=VECTOR('',#8852,5.6);
#2268=VECTOR('',#8861,10.);
#2269=VECTOR('',#8868,10.);
#2270=VECTOR('',#8873,10.);
#2271=VECTOR('',#8874,10.);
#2272=VECTOR('',#8879,10.);
#2273=VECTOR('',#8882,10.);
#2274=VECTOR('',#8883,10.);
#2275=VECTOR('',#8884,10.);
#2276=VECTOR('',#8891,0.625);
#2277=VECTOR('',#8896,1.25);
#2278=VECTOR('',#8903,1.25);
#2279=VECTOR('',#8908,1.25);
#2280=VECTOR('',#8917,5.6);
#2281=VECTOR('',#8922,6.);
#2282=VECTOR('',#8923,6.);
#2283=VECTOR('',#8928,5.6);
#2284=VECTOR('',#8941,12.15);
#2285=VECTOR('',#8976,8.3);
#2286=VECTOR('',#9089,11.7);
#2287=VECTOR('',#9098,8.3);
#2288=VECTOR('',#9119,13.85);
#2289=VECTOR('',#9124,14.);
#2290=VECTOR('',#9129,13.85);
#2291=VECTOR('',#9136,12.6);
#2292=VECTOR('',#9145,6.15);
#2293=VECTOR('',#9150,6.);
#2294=VECTOR('',#9155,6.15);
#2295=VECTOR('',#9172,8.55);
#2296=VECTOR('',#9179,11.65);
#2297=VECTOR('',#9190,13.85);
#2298=VECTOR('',#9195,14.);
#2299=VECTOR('',#9200,13.85);
#2300=VECTOR('',#9207,11.65);
#2301=VECTOR('',#9218,8.55);
#2302=VECTOR('',#9225,6.15);
#2303=VECTOR('',#9230,6.);
#2304=VECTOR('',#9235,6.15);
#2305=VECTOR('',#9242,9.);
#2306=VECTOR('',#9251,6.);
#2307=VECTOR('',#9260,2.);
#2308=VECTOR('',#9265,2.);
#2309=VECTOR('',#9268,2.);
#2310=VECTOR('',#9271,2.);
#2311=VECTOR('',#9274,2.);
#2312=VECTOR('',#9277,1.5555);
#2313=VECTOR('',#9282,1.5555);
#2314=VECTOR('',#9285,1.5555);
#2315=VECTOR('',#9288,1.5555);
#2316=VECTOR('',#9307,0.5);
#2317=VECTOR('',#9312,10.);
#2318=VECTOR('',#9313,10.);
#2319=VECTOR('',#9314,10.);
#2320=VECTOR('',#9315,10.);
#2321=VECTOR('',#9318,10.);
#2322=VECTOR('',#9319,10.);
#2323=VECTOR('',#9320,10.);
#2324=VECTOR('',#9323,10.);
#2325=VECTOR('',#9324,10.);
#2326=VECTOR('',#9325,10.);
#2327=VECTOR('',#9328,10.);
#2328=VECTOR('',#9329,10.);
#2329=VECTOR('',#9330,10.);
#2330=VECTOR('',#9333,10.);
#2331=VECTOR('',#9334,10.);
#2332=VECTOR('',#9335,10.);
#2333=VECTOR('',#9338,10.);
#2334=VECTOR('',#9339,10.);
#2335=VECTOR('',#9348,1.75);
#2336=VECTOR('',#9357,1.8);
#2337=VECTOR('',#9366,0.85);
#2338=VECTOR('',#9373,0.85);
#2339=VECTOR('',#9378,10.);
#2340=VECTOR('',#9381,10.);
#2341=VECTOR('',#9386,10.);
#2342=VECTOR('',#9387,10.);
#2343=VECTOR('',#9388,10.);
#2344=VECTOR('',#9391,10.);
#2345=VECTOR('',#9392,10.);
#2346=VECTOR('',#9393,10.);
#2347=VECTOR('',#9396,10.);
#2348=VECTOR('',#9397,10.);
#2349=VECTOR('',#9398,10.);
#2350=VECTOR('',#9401,10.);
#2351=VECTOR('',#9402,10.);
#2352=VECTOR('',#9405,10.);
#2353=VECTOR('',#9408,10.);
#2354=VECTOR('',#9409,10.);
#2355=VECTOR('',#9412,10.);
#2356=VECTOR('',#9413,10.);
#2357=VECTOR('',#9414,10.);
#2358=VECTOR('',#9417,10.);
#2359=CIRCLE('',#7149,14.);
#2360=CIRCLE('',#7150,14.);
#2361=CIRCLE('',#7152,14.7);
#2362=CIRCLE('',#7154,14.7);
#2363=CIRCLE('',#7156,14.);
#2364=CIRCLE('',#7158,14.);
#2365=CIRCLE('',#7160,12.);
#2366=CIRCLE('',#7162,12.);
#2367=CIRCLE('',#7164,14.);
#2368=CIRCLE('',#7166,14.);
#2369=CIRCLE('',#7168,14.);
#2370=CIRCLE('',#7169,14.);
#2371=CIRCLE('',#7171,14.7);
#2372=CIRCLE('',#7173,14.7);
#2373=CIRCLE('',#7175,14.);
#2374=CIRCLE('',#7177,14.);
#2375=CIRCLE('',#7179,12.);
#2376=CIRCLE('',#7181,12.);
#2377=CIRCLE('',#7183,12.);
#2378=CIRCLE('',#7184,12.);
#2379=CIRCLE('',#7186,14.);
#2380=CIRCLE('',#7188,14.);
#2381=CIRCLE('',#7190,14.7);
#2382=CIRCLE('',#7192,14.7);
#2383=CIRCLE('',#7194,14.);
#2384=CIRCLE('',#7196,14.);
#2385=CIRCLE('',#7198,20.);
#2386=CIRCLE('',#7199,1.5);
#2387=CIRCLE('',#7200,21.5);
#2388=CIRCLE('',#7201,20.);
#2389=CIRCLE('',#7203,20.);
#2390=CIRCLE('',#7204,20.);
#2391=CIRCLE('',#7206,1.2);
#2392=CIRCLE('',#7207,1.2);
#2393=CIRCLE('',#7208,1.2);
#2394=CIRCLE('',#7209,1.2);
#2395=CIRCLE('',#7211,19.);
#2396=CIRCLE('',#7215,2.);
#2397=CIRCLE('',#7218,2.);
#2398=CIRCLE('',#7221,2.);
#2399=CIRCLE('',#7224,2.);
#2400=CIRCLE('',#7226,2.);
#2401=CIRCLE('',#7229,2.);
#2402=CIRCLE('',#7232,1.);
#2403=CIRCLE('',#7235,2.);
#2404=CIRCLE('',#7236,1.);
#2405=CIRCLE('',#7239,2.);
#2406=CIRCLE('',#7240,1.);
#2407=CIRCLE('',#7243,1.);
#2408=CIRCLE('',#7246,4.);
#2409=CIRCLE('',#7247,4.);
#2410=CIRCLE('',#7248,4.);
#2411=CIRCLE('',#7249,4.);
#2412=CIRCLE('',#7251,3.);
#2413=CIRCLE('',#7254,3.);
#2414=CIRCLE('',#7257,3.);
#2415=CIRCLE('',#7260,3.);
#2416=CIRCLE('',#7264,3.);
#2417=CIRCLE('',#7267,3.);
#2418=CIRCLE('',#7269,3.);
#2419=CIRCLE('',#7270,3.);
#2420=CIRCLE('',#7281,9.16192731696939);
#2421=CIRCLE('',#7283,2.05);
#2422=CIRCLE('',#7286,2.05);
#2423=CIRCLE('',#7289,6.525);
#2424=CIRCLE('',#7290,6.025);
#2425=CIRCLE('',#7291,6.025);
#2426=CIRCLE('',#7293,6.025);
#2427=CIRCLE('',#7294,6.025);
#2428=CIRCLE('',#7296,9.16192731696939);
#2429=CIRCLE('',#7297,9.16192731696939);
#2430=CIRCLE('',#7298,9.16192731696939);
#2431=CIRCLE('',#7299,9.16192731696939);
#2432=CIRCLE('',#7300,9.16192731696939);
#2433=CIRCLE('',#7301,9.16192731696939);
#2434=CIRCLE('',#7302,9.16192731696939);
#2435=CIRCLE('',#7303,9.16192731696939);
#2436=CIRCLE('',#7304,9.16192731696939);
#2437=CIRCLE('',#7305,9.16192731696939);
#2438=CIRCLE('',#7306,9.16192731696939);
#2439=CIRCLE('',#7307,9.16192731696939);
#2440=CIRCLE('',#7308,9.16192731696939);
#2441=CIRCLE('',#7309,9.16192731696939);
#2442=CIRCLE('',#7310,9.16192731696939);
#2443=CIRCLE('',#7311,9.16192731696939);
#2444=CIRCLE('',#7312,9.16192731696939);
#2445=CIRCLE('',#7313,9.16192731696939);
#2446=CIRCLE('',#7314,9.16192731696939);
#2447=CIRCLE('',#7316,6.525);
#2448=CIRCLE('',#7318,9.5);
#2449=CIRCLE('',#7320,10.);
#2450=CIRCLE('',#7321,10.);
#2451=CIRCLE('',#7323,10.);
#2452=CIRCLE('',#7325,14.4466666666667);
#2453=CIRCLE('',#7327,14.4466666666667);
#2454=CIRCLE('',#7329,14.4466666666667);
#2455=CIRCLE('',#7331,14.4466666666667);
#2456=CIRCLE('',#7333,14.4466666666667);
#2457=CIRCLE('',#7335,14.4466666666667);
#2458=CIRCLE('',#7337,14.4466666666667);
#2459=CIRCLE('',#7339,14.4466666666667);
#2460=CIRCLE('',#7341,14.4466666666667);
#2461=CIRCLE('',#7343,14.4466666666667);
#2462=CIRCLE('',#7345,14.4466666666667);
#2463=CIRCLE('',#7347,14.4466666666667);
#2464=CIRCLE('',#7349,14.4466666666667);
#2465=CIRCLE('',#7351,14.4466666666667);
#2466=CIRCLE('',#7353,14.4466666666667);
#2467=CIRCLE('',#7355,14.4466666666667);
#2468=CIRCLE('',#7357,14.4466666666667);
#2469=CIRCLE('',#7359,14.4466666666667);
#2470=CIRCLE('',#7361,14.4466666666667);
#2471=CIRCLE('',#7363,14.4233723052509);
#2472=CIRCLE('',#7364,10.5);
#2473=CIRCLE('',#7366,10.5);
#2474=CIRCLE('',#7368,14.4466666666667);
#2475=CIRCLE('',#7370,14.4034641071566);
#2476=CIRCLE('',#7372,14.4034641071566);
#2477=CIRCLE('',#7373,14.4034641071566);
#2478=CIRCLE('',#7374,14.4034641071566);
#2479=CIRCLE('',#7375,14.4034641071566);
#2480=CIRCLE('',#7376,14.4034641071566);
#2481=CIRCLE('',#7377,14.4034641071566);
#2482=CIRCLE('',#7378,14.4034641071566);
#2483=CIRCLE('',#7379,14.4034641071566);
#2484=CIRCLE('',#7380,14.4034641071566);
#2485=CIRCLE('',#7381,14.4034641071566);
#2486=CIRCLE('',#7382,14.4034641071566);
#2487=CIRCLE('',#7383,14.4034641071566);
#2488=CIRCLE('',#7384,14.4034641071566);
#2489=CIRCLE('',#7385,14.4034641071566);
#2490=CIRCLE('',#7386,14.4034641071566);
#2491=CIRCLE('',#7387,14.4034641071566);
#2492=CIRCLE('',#7388,14.4034641071566);
#2493=CIRCLE('',#7389,14.4034641071566);
#2494=CIRCLE('',#7390,14.4034641071566);
#2495=CIRCLE('',#7391,14.4034641071566);
#2496=CIRCLE('',#7414,2.05);
#2497=CIRCLE('',#7417,2.05);
#2498=CIRCLE('',#7420,6.525);
#2499=CIRCLE('',#7421,6.025);
#2500=CIRCLE('',#7422,6.025);
#2501=CIRCLE('',#7424,6.025);
#2502=CIRCLE('',#7425,6.025);
#2503=CIRCLE('',#7427,9.16192731696939);
#2504=CIRCLE('',#7428,9.16192731696939);
#2505=CIRCLE('',#7429,9.16192731696939);
#2506=CIRCLE('',#7430,9.16192731696939);
#2507=CIRCLE('',#7431,9.16192731696939);
#2508=CIRCLE('',#7432,9.16192731696939);
#2509=CIRCLE('',#7433,9.16192731696939);
#2510=CIRCLE('',#7434,9.16192731696939);
#2511=CIRCLE('',#7435,9.16192731696939);
#2512=CIRCLE('',#7436,9.16192731696939);
#2513=CIRCLE('',#7437,9.16192731696939);
#2514=CIRCLE('',#7438,9.16192731696939);
#2515=CIRCLE('',#7439,9.16192731696939);
#2516=CIRCLE('',#7440,9.16192731696939);
#2517=CIRCLE('',#7441,9.16192731696939);
#2518=CIRCLE('',#7442,9.16192731696939);
#2519=CIRCLE('',#7443,9.16192731696939);
#2520=CIRCLE('',#7444,9.16192731696939);
#2521=CIRCLE('',#7445,9.16192731696939);
#2522=CIRCLE('',#7446,9.16192731696939);
#2523=CIRCLE('',#7448,6.525);
#2524=CIRCLE('',#7450,9.5);
#2525=CIRCLE('',#7452,10.);
#2526=CIRCLE('',#7453,10.);
#2527=CIRCLE('',#7455,10.);
#2528=CIRCLE('',#7457,14.4466666666667);
#2529=CIRCLE('',#7459,14.4466666666667);
#2530=CIRCLE('',#7461,14.4466666666667);
#2531=CIRCLE('',#7463,14.4466666666667);
#2532=CIRCLE('',#7465,14.4466666666667);
#2533=CIRCLE('',#7467,14.4466666666667);
#2534=CIRCLE('',#7469,14.4466666666667);
#2535=CIRCLE('',#7471,14.4466666666667);
#2536=CIRCLE('',#7473,14.4466666666667);
#2537=CIRCLE('',#7475,14.4466666666667);
#2538=CIRCLE('',#7477,14.4466666666667);
#2539=CIRCLE('',#7479,14.4466666666667);
#2540=CIRCLE('',#7481,14.4466666666667);
#2541=CIRCLE('',#7483,14.4466666666667);
#2542=CIRCLE('',#7485,14.4466666666667);
#2543=CIRCLE('',#7487,14.4466666666667);
#2544=CIRCLE('',#7489,14.4466666666667);
#2545=CIRCLE('',#7491,14.4466666666667);
#2546=CIRCLE('',#7493,14.4466666666667);
#2547=CIRCLE('',#7495,14.4233723052509);
#2548=CIRCLE('',#7496,10.5);
#2549=CIRCLE('',#7498,10.5);
#2550=CIRCLE('',#7500,14.4466666666667);
#2551=CIRCLE('',#7502,14.4034641071566);
#2552=CIRCLE('',#7504,14.4034641071566);
#2553=CIRCLE('',#7505,14.4034641071566);
#2554=CIRCLE('',#7506,14.4034641071566);
#2555=CIRCLE('',#7507,14.4034641071566);
#2556=CIRCLE('',#7508,14.4034641071566);
#2557=CIRCLE('',#7509,14.4034641071566);
#2558=CIRCLE('',#7510,14.4034641071566);
#2559=CIRCLE('',#7511,14.4034641071566);
#2560=CIRCLE('',#7512,14.4034641071566);
#2561=CIRCLE('',#7513,14.4034641071566);
#2562=CIRCLE('',#7514,14.4034641071566);
#2563=CIRCLE('',#7515,14.4034641071566);
#2564=CIRCLE('',#7516,14.4034641071566);
#2565=CIRCLE('',#7517,14.4034641071566);
#2566=CIRCLE('',#7518,14.4034641071566);
#2567=CIRCLE('',#7519,14.4034641071566);
#2568=CIRCLE('',#7520,14.4034641071566);
#2569=CIRCLE('',#7521,14.4034641071566);
#2570=CIRCLE('',#7522,14.4034641071566);
#2571=CIRCLE('',#7523,14.4034641071566);
#2572=CIRCLE('',#7546,6.);
#2573=CIRCLE('',#7547,6.);
#2574=CIRCLE('',#7549,6.);
#2575=CIRCLE('',#7550,6.);
#2576=CIRCLE('',#7553,6.);
#2577=CIRCLE('',#7556,6.);
#2578=CIRCLE('',#7558,1.25);
#2579=CIRCLE('',#7560,1.25);
#2580=CIRCLE('',#7562,1.25);
#2581=CIRCLE('',#7563,1.25);
#2582=CIRCLE('',#7566,5.2);
#2583=CIRCLE('',#7568,6.);
#2584=CIRCLE('',#7570,6.);
#2585=CIRCLE('',#7572,5.2);
#2586=CIRCLE('',#7576,6.);
#2587=CIRCLE('',#7577,6.);
#2588=CIRCLE('',#7579,6.);
#2589=CIRCLE('',#7580,6.);
#2590=CIRCLE('',#7583,6.);
#2591=CIRCLE('',#7586,6.);
#2592=CIRCLE('',#7588,1.25);
#2593=CIRCLE('',#7590,1.25);
#2594=CIRCLE('',#7592,1.25);
#2595=CIRCLE('',#7593,1.25);
#2596=CIRCLE('',#7596,5.2);
#2597=CIRCLE('',#7598,6.);
#2598=CIRCLE('',#7600,6.);
#2599=CIRCLE('',#7602,5.2);
#2600=CIRCLE('',#7606,2.38125);
#2601=CIRCLE('',#7608,12.6);
#2602=CIRCLE('',#7609,11.7);
#2603=CIRCLE('',#7610,11.7);
#2604=CIRCLE('',#7611,11.7);
#2605=CIRCLE('',#7612,11.7);
#2606=CIRCLE('',#7613,11.7);
#2607=CIRCLE('',#7614,11.7);
#2608=CIRCLE('',#7615,11.7);
#2609=CIRCLE('',#7616,11.7);
#2610=CIRCLE('',#7617,11.7);
#2611=CIRCLE('',#7618,11.7);
#2612=CIRCLE('',#7620,11.7);
#2613=CIRCLE('',#7622,8.3);
#2614=CIRCLE('',#7623,8.3);
#2615=CIRCLE('',#7624,8.3);
#2616=CIRCLE('',#7625,8.3);
#2617=CIRCLE('',#7626,8.3);
#2618=CIRCLE('',#7627,8.3);
#2619=CIRCLE('',#7628,8.3);
#2620=CIRCLE('',#7629,8.3);
#2621=CIRCLE('',#7630,8.3);
#2622=CIRCLE('',#7631,8.3);
#2623=CIRCLE('',#7632,8.3);
#2624=CIRCLE('',#7634,8.3);
#2625=CIRCLE('',#7636,2.38125);
#2626=CIRCLE('',#7638,11.7);
#2627=CIRCLE('',#7640,8.3);
#2628=CIRCLE('',#7642,2.38125);
#2629=CIRCLE('',#7644,11.7);
#2630=CIRCLE('',#7646,8.3);
#2631=CIRCLE('',#7648,2.38125);
#2632=CIRCLE('',#7650,11.7);
#2633=CIRCLE('',#7652,8.3);
#2634=CIRCLE('',#7654,2.38125);
#2635=CIRCLE('',#7656,11.7);
#2636=CIRCLE('',#7658,8.3);
#2637=CIRCLE('',#7660,2.38125);
#2638=CIRCLE('',#7662,11.7);
#2639=CIRCLE('',#7664,8.3);
#2640=CIRCLE('',#7666,2.38125);
#2641=CIRCLE('',#7668,11.7);
#2642=CIRCLE('',#7670,8.3);
#2643=CIRCLE('',#7672,2.38125);
#2644=CIRCLE('',#7674,11.7);
#2645=CIRCLE('',#7676,8.3);
#2646=CIRCLE('',#7678,2.38125);
#2647=CIRCLE('',#7680,11.7);
#2648=CIRCLE('',#7681,11.7);
#2649=CIRCLE('',#7682,11.7);
#2650=CIRCLE('',#7685,8.3);
#2651=CIRCLE('',#7686,8.3);
#2652=CIRCLE('',#7687,8.3);
#2653=CIRCLE('',#7690,2.38125);
#2654=CIRCLE('',#7693,13.7);
#2655=CIRCLE('',#7695,14.);
#2656=CIRCLE('',#7697,14.);
#2657=CIRCLE('',#7699,13.7);
#2658=CIRCLE('',#7701,12.6);
#2659=CIRCLE('',#7705,6.3);
#2660=CIRCLE('',#7707,6.);
#2661=CIRCLE('',#7709,6.);
#2662=CIRCLE('',#7711,6.3);
#2663=CIRCLE('',#7715,8.4);
#2664=CIRCLE('',#7716,6.3);
#2665=CIRCLE('',#7718,8.7);
#2666=CIRCLE('',#7720,11.5);
#2667=CIRCLE('',#7722,11.8);
#2668=CIRCLE('',#7724,13.7);
#2669=CIRCLE('',#7726,14.);
#2670=CIRCLE('',#7728,14.);
#2671=CIRCLE('',#7730,13.7);
#2672=CIRCLE('',#7732,11.8);
#2673=CIRCLE('',#7734,11.5);
#2674=CIRCLE('',#7736,8.7);
#2675=CIRCLE('',#7738,8.4);
#2676=CIRCLE('',#7740,6.3);
#2677=CIRCLE('',#7742,6.);
#2678=CIRCLE('',#7744,6.);
#2679=CIRCLE('',#7748,9.);
#2680=CIRCLE('',#7749,9.);
#2681=CIRCLE('',#7751,6.);
#2682=CIRCLE('',#7753,6.);
#2683=CIRCLE('',#7757,1.954);
#2684=CIRCLE('',#7763,1.5555);
#2685=CIRCLE('',#7768,1.954);
#2686=CIRCLE('',#7769,1.954);
#2687=CIRCLE('',#7771,1.954);
#2688=CIRCLE('',#7772,1.954);
#2689=CIRCLE('',#7773,1.5555);
#2690=CIRCLE('',#7776,0.98360655737705);
#2691=CIRCLE('',#7785,1.5);
#2692=CIRCLE('',#7788,1.954);
#2693=CIRCLE('',#7790,1.6);
#2694=CIRCLE('',#7794,0.85);
#2695=CIRCLE('',#7795,0.85);
#2696=CIRCLE('',#7797,0.85);
#2697=CIRCLE('',#7798,0.85);
#2698=CIRCLE('',#7800,14.7);
#2699=CIRCLE('',#7801,14.7);
#2700=CIRCLE('',#7803,12.4);
#2701=CIRCLE('',#7811,12.4);
#2702=VERTEX_POINT('',#9463);
#2703=VERTEX_POINT('',#9465);
#2704=VERTEX_POINT('',#9469);
#2705=VERTEX_POINT('',#9472);
#2706=VERTEX_POINT('',#9476);
#2707=VERTEX_POINT('',#9479);
#2708=VERTEX_POINT('',#9483);
#2709=VERTEX_POINT('',#9486);
#2710=VERTEX_POINT('',#9490);
#2711=VERTEX_POINT('',#9493);
#2712=VERTEX_POINT('',#9497);
#2713=VERTEX_POINT('',#9499);
#2714=VERTEX_POINT('',#9503);
#2715=VERTEX_POINT('',#9506);
#2716=VERTEX_POINT('',#9510);
#2717=VERTEX_POINT('',#9513);
#2718=VERTEX_POINT('',#9517);
#2719=VERTEX_POINT('',#9520);
#2720=VERTEX_POINT('',#9524);
#2721=VERTEX_POINT('',#9526);
#2722=VERTEX_POINT('',#9530);
#2723=VERTEX_POINT('',#9533);
#2724=VERTEX_POINT('',#9537);
#2725=VERTEX_POINT('',#9540);
#2726=VERTEX_POINT('',#9544);
#2727=VERTEX_POINT('',#9547);
#2728=VERTEX_POINT('',#9551);
#2729=VERTEX_POINT('',#9552);
#2730=VERTEX_POINT('',#9554);
#2731=VERTEX_POINT('',#9559);
#2732=VERTEX_POINT('',#9561);
#2733=VERTEX_POINT('',#9565);
#2734=VERTEX_POINT('',#9566);
#2735=VERTEX_POINT('',#9568);
#2736=VERTEX_POINT('',#9570);
#2737=VERTEX_POINT('',#9572);
#2738=VERTEX_POINT('',#9574);
#2739=VERTEX_POINT('',#9576);
#2740=VERTEX_POINT('',#9578);
#2741=VERTEX_POINT('',#9582);
#2742=VERTEX_POINT('',#9587);
#2743=VERTEX_POINT('',#9589);
#2744=VERTEX_POINT('',#9593);
#2745=VERTEX_POINT('',#9597);
#2746=VERTEX_POINT('',#9601);
#2747=VERTEX_POINT('',#9605);
#2748=VERTEX_POINT('',#9609);
#2749=VERTEX_POINT('',#9613);
#2750=VERTEX_POINT('',#9619);
#2751=VERTEX_POINT('',#9621);
#2752=VERTEX_POINT('',#9625);
#2753=VERTEX_POINT('',#9629);
#2754=VERTEX_POINT('',#9633);
#2755=VERTEX_POINT('',#9637);
#2756=VERTEX_POINT('',#9639);
#2757=VERTEX_POINT('',#9643);
#2758=VERTEX_POINT('',#9644);
#2759=VERTEX_POINT('',#9649);
#2760=VERTEX_POINT('',#9650);
#2761=VERTEX_POINT('',#9655);
#2762=VERTEX_POINT('',#9657);
#2763=VERTEX_POINT('',#9661);
#2764=VERTEX_POINT('',#9666);
#2765=VERTEX_POINT('',#9670);
#2766=VERTEX_POINT('',#9676);
#2767=VERTEX_POINT('',#9677);
#2768=VERTEX_POINT('',#9679);
#2769=VERTEX_POINT('',#9681);
#2770=VERTEX_POINT('',#9683);
#2771=VERTEX_POINT('',#9685);
#2772=VERTEX_POINT('',#9687);
#2773=VERTEX_POINT('',#9689);
#2774=VERTEX_POINT('',#9693);
#2775=VERTEX_POINT('',#9695);
#2776=VERTEX_POINT('',#9699);
#2777=VERTEX_POINT('',#9703);
#2778=VERTEX_POINT('',#9707);
#2779=VERTEX_POINT('',#9711);
#2780=VERTEX_POINT('',#9715);
#2781=VERTEX_POINT('',#9719);
#2782=VERTEX_POINT('',#9725);
#2783=VERTEX_POINT('',#9727);
#2784=VERTEX_POINT('',#9731);
#2785=VERTEX_POINT('',#9735);
#2786=VERTEX_POINT('',#9739);
#2787=VERTEX_POINT('',#9743);
#2788=VERTEX_POINT('',#9745);
#2789=VERTEX_POINT('',#9747);
#2790=VERTEX_POINT('',#9766);
#2791=VERTEX_POINT('',#9767);
#2792=VERTEX_POINT('',#9769);
#2793=VERTEX_POINT('',#9776);
#2794=VERTEX_POINT('',#9783);
#2795=VERTEX_POINT('',#9784);
#2796=VERTEX_POINT('',#9795);
#2797=VERTEX_POINT('',#9825);
#2798=VERTEX_POINT('',#9829);
#2799=VERTEX_POINT('',#9831);
#2800=VERTEX_POINT('',#9842);
#2801=VERTEX_POINT('',#9872);
#2802=VERTEX_POINT('',#9873);
#2803=VERTEX_POINT('',#9892);
#2804=VERTEX_POINT('',#9915);
#2805=VERTEX_POINT('',#9917);
#2806=VERTEX_POINT('',#9955);
#2807=VERTEX_POINT('',#9957);
#2808=VERTEX_POINT('',#9959);
#2809=VERTEX_POINT('',#9963);
#2810=VERTEX_POINT('',#9964);
#2811=VERTEX_POINT('',#9970);
#2812=VERTEX_POINT('',#9971);
#2813=VERTEX_POINT('',#9973);
#2814=VERTEX_POINT('',#10009);
#2815=VERTEX_POINT('',#10045);
#2816=VERTEX_POINT('',#10047);
#2817=VERTEX_POINT('',#10083);
#2818=VERTEX_POINT('',#10119);
#2819=VERTEX_POINT('',#10121);
#2820=VERTEX_POINT('',#10157);
#2821=VERTEX_POINT('',#10193);
#2822=VERTEX_POINT('',#10195);
#2823=VERTEX_POINT('',#10231);
#2824=VERTEX_POINT('',#10267);
#2825=VERTEX_POINT('',#10269);
#2826=VERTEX_POINT('',#10305);
#2827=VERTEX_POINT('',#10341);
#2828=VERTEX_POINT('',#10343);
#2829=VERTEX_POINT('',#10379);
#2830=VERTEX_POINT('',#10415);
#2831=VERTEX_POINT('',#10417);
#2832=VERTEX_POINT('',#10453);
#2833=VERTEX_POINT('',#10489);
#2834=VERTEX_POINT('',#10491);
#2835=VERTEX_POINT('',#10527);
#2836=VERTEX_POINT('',#10563);
#2837=VERTEX_POINT('',#10565);
#2838=VERTEX_POINT('',#10636);
#2839=VERTEX_POINT('',#10672);
#2840=VERTEX_POINT('',#10708);
#2841=VERTEX_POINT('',#10710);
#2842=VERTEX_POINT('',#10746);
#2843=VERTEX_POINT('',#10782);
#2844=VERTEX_POINT('',#10784);
#2845=VERTEX_POINT('',#10820);
#2846=VERTEX_POINT('',#10856);
#2847=VERTEX_POINT('',#10858);
#2848=VERTEX_POINT('',#10894);
#2849=VERTEX_POINT('',#10930);
#2850=VERTEX_POINT('',#10932);
#2851=VERTEX_POINT('',#10968);
#2852=VERTEX_POINT('',#11004);
#2853=VERTEX_POINT('',#11006);
#2854=VERTEX_POINT('',#11042);
#2855=VERTEX_POINT('',#11078);
#2856=VERTEX_POINT('',#11080);
#2857=VERTEX_POINT('',#11116);
#2858=VERTEX_POINT('',#11152);
#2859=VERTEX_POINT('',#11154);
#2860=VERTEX_POINT('',#11190);
#2861=VERTEX_POINT('',#11226);
#2862=VERTEX_POINT('',#11228);
#2863=VERTEX_POINT('',#11264);
#2864=VERTEX_POINT('',#11300);
#2865=VERTEX_POINT('',#11302);
#2866=VERTEX_POINT('',#11338);
#2867=VERTEX_POINT('',#11374);
#2868=VERTEX_POINT('',#11376);
#2869=VERTEX_POINT('',#11448);
#2870=VERTEX_POINT('',#11452);
#2871=VERTEX_POINT('',#11455);
#2872=VERTEX_POINT('',#11457);
#2873=VERTEX_POINT('',#11462);
#2874=VERTEX_POINT('',#11466);
#2875=VERTEX_POINT('',#11467);
#2876=VERTEX_POINT('',#11484);
#2877=VERTEX_POINT('',#11497);
#2878=VERTEX_POINT('',#11498);
#2879=VERTEX_POINT('',#11515);
#2880=VERTEX_POINT('',#11528);
#2881=VERTEX_POINT('',#11529);
#2882=VERTEX_POINT('',#11546);
#2883=VERTEX_POINT('',#11559);
#2884=VERTEX_POINT('',#11560);
#2885=VERTEX_POINT('',#11577);
#2886=VERTEX_POINT('',#11590);
#2887=VERTEX_POINT('',#11591);
#2888=VERTEX_POINT('',#11608);
#2889=VERTEX_POINT('',#11621);
#2890=VERTEX_POINT('',#11622);
#2891=VERTEX_POINT('',#11639);
#2892=VERTEX_POINT('',#11652);
#2893=VERTEX_POINT('',#11653);
#2894=VERTEX_POINT('',#11670);
#2895=VERTEX_POINT('',#11683);
#2896=VERTEX_POINT('',#11684);
#2897=VERTEX_POINT('',#11701);
#2898=VERTEX_POINT('',#11714);
#2899=VERTEX_POINT('',#11715);
#2900=VERTEX_POINT('',#11732);
#2901=VERTEX_POINT('',#11745);
#2902=VERTEX_POINT('',#11746);
#2903=VERTEX_POINT('',#11763);
#2904=VERTEX_POINT('',#11776);
#2905=VERTEX_POINT('',#11777);
#2906=VERTEX_POINT('',#11794);
#2907=VERTEX_POINT('',#11807);
#2908=VERTEX_POINT('',#11808);
#2909=VERTEX_POINT('',#11825);
#2910=VERTEX_POINT('',#11838);
#2911=VERTEX_POINT('',#11839);
#2912=VERTEX_POINT('',#11856);
#2913=VERTEX_POINT('',#11869);
#2914=VERTEX_POINT('',#11870);
#2915=VERTEX_POINT('',#11887);
#2916=VERTEX_POINT('',#11900);
#2917=VERTEX_POINT('',#11901);
#2918=VERTEX_POINT('',#11918);
#2919=VERTEX_POINT('',#11931);
#2920=VERTEX_POINT('',#11932);
#2921=VERTEX_POINT('',#11949);
#2922=VERTEX_POINT('',#11962);
#2923=VERTEX_POINT('',#11963);
#2924=VERTEX_POINT('',#11980);
#2925=VERTEX_POINT('',#11993);
#2926=VERTEX_POINT('',#11994);
#2927=VERTEX_POINT('',#12011);
#2928=VERTEX_POINT('',#12024);
#2929=VERTEX_POINT('',#12025);
#2930=VERTEX_POINT('',#12042);
#2931=VERTEX_POINT('',#12055);
#2932=VERTEX_POINT('',#12057);
#2933=VERTEX_POINT('',#12061);
#2934=VERTEX_POINT('',#12065);
#2935=VERTEX_POINT('',#12066);
#2936=VERTEX_POINT('',#12083);
#2937=VERTEX_POINT('',#12120);
#2938=VERTEX_POINT('',#12180);
#2939=VERTEX_POINT('',#12240);
#2940=VERTEX_POINT('',#12300);
#2941=VERTEX_POINT('',#12360);
#2942=VERTEX_POINT('',#12420);
#2943=VERTEX_POINT('',#12480);
#2944=VERTEX_POINT('',#12540);
#2945=VERTEX_POINT('',#12600);
#2946=VERTEX_POINT('',#12660);
#2947=VERTEX_POINT('',#12720);
#2948=VERTEX_POINT('',#12756);
#2949=VERTEX_POINT('',#12816);
#2950=VERTEX_POINT('',#12876);
#2951=VERTEX_POINT('',#12936);
#2952=VERTEX_POINT('',#12996);
#2953=VERTEX_POINT('',#13056);
#2954=VERTEX_POINT('',#13116);
#2955=VERTEX_POINT('',#13176);
#2956=VERTEX_POINT('',#13236);
#2957=VERTEX_POINT('',#13381);
#2958=VERTEX_POINT('',#13431);
#2959=VERTEX_POINT('',#13434);
#2960=VERTEX_POINT('',#13442);
#2961=VERTEX_POINT('',#13472);
#2962=VERTEX_POINT('',#13514);
#2963=VERTEX_POINT('',#13556);
#2964=VERTEX_POINT('',#13598);
#2965=VERTEX_POINT('',#13628);
#2966=VERTEX_POINT('',#13658);
#2967=VERTEX_POINT('',#13700);
#2968=VERTEX_POINT('',#13742);
#2969=VERTEX_POINT('',#13772);
#2970=VERTEX_POINT('',#13802);
#2971=VERTEX_POINT('',#13844);
#2972=VERTEX_POINT('',#13886);
#2973=VERTEX_POINT('',#13928);
#2974=VERTEX_POINT('',#13958);
#2975=VERTEX_POINT('',#13988);
#2976=VERTEX_POINT('',#14030);
#2977=VERTEX_POINT('',#14072);
#2978=VERTEX_POINT('',#15844);
#2979=VERTEX_POINT('',#15845);
#2980=VERTEX_POINT('',#15856);
#2981=VERTEX_POINT('',#15886);
#2982=VERTEX_POINT('',#15890);
#2983=VERTEX_POINT('',#15892);
#2984=VERTEX_POINT('',#15903);
#2985=VERTEX_POINT('',#15933);
#2986=VERTEX_POINT('',#15934);
#2987=VERTEX_POINT('',#15953);
#2988=VERTEX_POINT('',#15976);
#2989=VERTEX_POINT('',#15978);
#2990=VERTEX_POINT('',#16016);
#2991=VERTEX_POINT('',#16018);
#2992=VERTEX_POINT('',#16020);
#2993=VERTEX_POINT('',#16024);
#2994=VERTEX_POINT('',#16025);
#2995=VERTEX_POINT('',#16031);
#2996=VERTEX_POINT('',#16032);
#2997=VERTEX_POINT('',#16034);
#2998=VERTEX_POINT('',#16070);
#2999=VERTEX_POINT('',#16106);
#3000=VERTEX_POINT('',#16108);
#3001=VERTEX_POINT('',#16144);
#3002=VERTEX_POINT('',#16180);
#3003=VERTEX_POINT('',#16182);
#3004=VERTEX_POINT('',#16218);
#3005=VERTEX_POINT('',#16254);
#3006=VERTEX_POINT('',#16256);
#3007=VERTEX_POINT('',#16292);
#3008=VERTEX_POINT('',#16328);
#3009=VERTEX_POINT('',#16330);
#3010=VERTEX_POINT('',#16366);
#3011=VERTEX_POINT('',#16402);
#3012=VERTEX_POINT('',#16404);
#3013=VERTEX_POINT('',#16440);
#3014=VERTEX_POINT('',#16476);
#3015=VERTEX_POINT('',#16478);
#3016=VERTEX_POINT('',#16514);
#3017=VERTEX_POINT('',#16550);
#3018=VERTEX_POINT('',#16552);
#3019=VERTEX_POINT('',#16588);
#3020=VERTEX_POINT('',#16624);
#3021=VERTEX_POINT('',#16626);
#3022=VERTEX_POINT('',#16662);
#3023=VERTEX_POINT('',#16698);
#3024=VERTEX_POINT('',#16700);
#3025=VERTEX_POINT('',#16736);
#3026=VERTEX_POINT('',#16772);
#3027=VERTEX_POINT('',#16774);
#3028=VERTEX_POINT('',#16810);
#3029=VERTEX_POINT('',#16846);
#3030=VERTEX_POINT('',#16848);
#3031=VERTEX_POINT('',#16884);
#3032=VERTEX_POINT('',#16920);
#3033=VERTEX_POINT('',#16922);
#3034=VERTEX_POINT('',#16958);
#3035=VERTEX_POINT('',#16994);
#3036=VERTEX_POINT('',#16996);
#3037=VERTEX_POINT('',#17032);
#3038=VERTEX_POINT('',#17068);
#3039=VERTEX_POINT('',#17070);
#3040=VERTEX_POINT('',#17106);
#3041=VERTEX_POINT('',#17142);
#3042=VERTEX_POINT('',#17144);
#3043=VERTEX_POINT('',#17180);
#3044=VERTEX_POINT('',#17216);
#3045=VERTEX_POINT('',#17218);
#3046=VERTEX_POINT('',#17254);
#3047=VERTEX_POINT('',#17290);
#3048=VERTEX_POINT('',#17292);
#3049=VERTEX_POINT('',#17328);
#3050=VERTEX_POINT('',#17364);
#3051=VERTEX_POINT('',#17366);
#3052=VERTEX_POINT('',#17402);
#3053=VERTEX_POINT('',#17438);
#3054=VERTEX_POINT('',#17440);
#3055=VERTEX_POINT('',#17512);
#3056=VERTEX_POINT('',#17516);
#3057=VERTEX_POINT('',#17519);
#3058=VERTEX_POINT('',#17521);
#3059=VERTEX_POINT('',#17526);
#3060=VERTEX_POINT('',#17530);
#3061=VERTEX_POINT('',#17531);
#3062=VERTEX_POINT('',#17546);
#3063=VERTEX_POINT('',#17559);
#3064=VERTEX_POINT('',#17560);
#3065=VERTEX_POINT('',#17575);
#3066=VERTEX_POINT('',#17588);
#3067=VERTEX_POINT('',#17589);
#3068=VERTEX_POINT('',#17604);
#3069=VERTEX_POINT('',#17617);
#3070=VERTEX_POINT('',#17618);
#3071=VERTEX_POINT('',#17633);
#3072=VERTEX_POINT('',#17646);
#3073=VERTEX_POINT('',#17647);
#3074=VERTEX_POINT('',#17662);
#3075=VERTEX_POINT('',#17675);
#3076=VERTEX_POINT('',#17676);
#3077=VERTEX_POINT('',#17691);
#3078=VERTEX_POINT('',#17704);
#3079=VERTEX_POINT('',#17705);
#3080=VERTEX_POINT('',#17720);
#3081=VERTEX_POINT('',#17733);
#3082=VERTEX_POINT('',#17734);
#3083=VERTEX_POINT('',#17749);
#3084=VERTEX_POINT('',#17762);
#3085=VERTEX_POINT('',#17763);
#3086=VERTEX_POINT('',#17778);
#3087=VERTEX_POINT('',#17791);
#3088=VERTEX_POINT('',#17792);
#3089=VERTEX_POINT('',#17807);
#3090=VERTEX_POINT('',#17820);
#3091=VERTEX_POINT('',#17821);
#3092=VERTEX_POINT('',#17836);
#3093=VERTEX_POINT('',#17849);
#3094=VERTEX_POINT('',#17850);
#3095=VERTEX_POINT('',#17865);
#3096=VERTEX_POINT('',#17878);
#3097=VERTEX_POINT('',#17879);
#3098=VERTEX_POINT('',#17894);
#3099=VERTEX_POINT('',#17907);
#3100=VERTEX_POINT('',#17908);
#3101=VERTEX_POINT('',#17923);
#3102=VERTEX_POINT('',#17936);
#3103=VERTEX_POINT('',#17937);
#3104=VERTEX_POINT('',#17952);
#3105=VERTEX_POINT('',#17965);
#3106=VERTEX_POINT('',#17966);
#3107=VERTEX_POINT('',#17981);
#3108=VERTEX_POINT('',#17994);
#3109=VERTEX_POINT('',#17995);
#3110=VERTEX_POINT('',#18010);
#3111=VERTEX_POINT('',#18023);
#3112=VERTEX_POINT('',#18024);
#3113=VERTEX_POINT('',#18039);
#3114=VERTEX_POINT('',#18052);
#3115=VERTEX_POINT('',#18053);
#3116=VERTEX_POINT('',#18068);
#3117=VERTEX_POINT('',#18081);
#3118=VERTEX_POINT('',#18083);
#3119=VERTEX_POINT('',#18087);
#3120=VERTEX_POINT('',#18091);
#3121=VERTEX_POINT('',#18092);
#3122=VERTEX_POINT('',#18107);
#3123=VERTEX_POINT('',#18144);
#3124=VERTEX_POINT('',#18204);
#3125=VERTEX_POINT('',#18264);
#3126=VERTEX_POINT('',#18324);
#3127=VERTEX_POINT('',#18384);
#3128=VERTEX_POINT('',#18444);
#3129=VERTEX_POINT('',#18504);
#3130=VERTEX_POINT('',#18564);
#3131=VERTEX_POINT('',#18624);
#3132=VERTEX_POINT('',#18684);
#3133=VERTEX_POINT('',#18744);
#3134=VERTEX_POINT('',#18804);
#3135=VERTEX_POINT('',#18864);
#3136=VERTEX_POINT('',#18924);
#3137=VERTEX_POINT('',#18984);
#3138=VERTEX_POINT('',#19044);
#3139=VERTEX_POINT('',#19104);
#3140=VERTEX_POINT('',#19164);
#3141=VERTEX_POINT('',#19224);
#3142=VERTEX_POINT('',#19284);
#3143=VERTEX_POINT('',#19363);
#3144=VERTEX_POINT('',#19401);
#3145=VERTEX_POINT('',#19404);
#3146=VERTEX_POINT('',#19434);
#3147=VERTEX_POINT('',#19464);
#3148=VERTEX_POINT('',#19494);
#3149=VERTEX_POINT('',#19524);
#3150=VERTEX_POINT('',#19554);
#3151=VERTEX_POINT('',#19584);
#3152=VERTEX_POINT('',#19614);
#3153=VERTEX_POINT('',#19644);
#3154=VERTEX_POINT('',#19674);
#3155=VERTEX_POINT('',#19704);
#3156=VERTEX_POINT('',#19734);
#3157=VERTEX_POINT('',#19764);
#3158=VERTEX_POINT('',#19794);
#3159=VERTEX_POINT('',#19824);
#3160=VERTEX_POINT('',#19854);
#3161=VERTEX_POINT('',#19884);
#3162=VERTEX_POINT('',#19914);
#3163=VERTEX_POINT('',#19944);
#3164=VERTEX_POINT('',#20978);
#3165=VERTEX_POINT('',#20979);
#3166=VERTEX_POINT('',#20981);
#3167=VERTEX_POINT('',#20985);
#3168=VERTEX_POINT('',#20986);
#3169=VERTEX_POINT('',#20988);
#3170=VERTEX_POINT('',#20995);
#3171=VERTEX_POINT('',#20996);
#3172=VERTEX_POINT('',#21000);
#3173=VERTEX_POINT('',#21002);
#3174=VERTEX_POINT('',#21008);
#3175=VERTEX_POINT('',#21009);
#3176=VERTEX_POINT('',#21013);
#3177=VERTEX_POINT('',#21017);
#3178=VERTEX_POINT('',#21019);
#3179=VERTEX_POINT('',#21023);
#3180=VERTEX_POINT('',#21026);
#3181=VERTEX_POINT('',#21029);
#3182=VERTEX_POINT('',#21033);
#3183=VERTEX_POINT('',#21038);
#3184=VERTEX_POINT('',#21044);
#3185=VERTEX_POINT('',#21045);
#3186=VERTEX_POINT('',#21047);
#3187=VERTEX_POINT('',#21051);
#3188=VERTEX_POINT('',#21052);
#3189=VERTEX_POINT('',#21054);
#3190=VERTEX_POINT('',#21061);
#3191=VERTEX_POINT('',#21062);
#3192=VERTEX_POINT('',#21066);
#3193=VERTEX_POINT('',#21068);
#3194=VERTEX_POINT('',#21074);
#3195=VERTEX_POINT('',#21075);
#3196=VERTEX_POINT('',#21079);
#3197=VERTEX_POINT('',#21083);
#3198=VERTEX_POINT('',#21085);
#3199=VERTEX_POINT('',#21089);
#3200=VERTEX_POINT('',#21092);
#3201=VERTEX_POINT('',#21095);
#3202=VERTEX_POINT('',#21099);
#3203=VERTEX_POINT('',#21104);
#3204=VERTEX_POINT('',#21110);
#3205=VERTEX_POINT('',#21111);
#3206=VERTEX_POINT('',#21113);
#3207=VERTEX_POINT('',#21114);
#3208=VERTEX_POINT('',#21121);
#3209=VERTEX_POINT('',#21133);
#3210=VERTEX_POINT('',#21151);
#3211=VERTEX_POINT('',#21152);
#3212=VERTEX_POINT('',#21159);
#3213=VERTEX_POINT('',#21170);
#3214=VERTEX_POINT('',#21188);
#3215=VERTEX_POINT('',#21190);
#3216=VERTEX_POINT('',#21192);
#3217=VERTEX_POINT('',#21197);
#3218=VERTEX_POINT('',#21199);
#3219=VERTEX_POINT('',#21206);
#3220=VERTEX_POINT('',#21208);
#3221=VERTEX_POINT('',#21215);
#3222=VERTEX_POINT('',#21217);
#3223=VERTEX_POINT('',#21224);
#3224=VERTEX_POINT('',#21226);
#3225=VERTEX_POINT('',#21233);
#3226=VERTEX_POINT('',#21235);
#3227=VERTEX_POINT('',#21243);
#3228=VERTEX_POINT('',#21245);
#3229=VERTEX_POINT('',#21252);
#3230=VERTEX_POINT('',#21254);
#3231=VERTEX_POINT('',#21261);
#3232=VERTEX_POINT('',#21263);
#3233=VERTEX_POINT('',#21270);
#3234=VERTEX_POINT('',#21277);
#3235=VERTEX_POINT('',#21291);
#3236=VERTEX_POINT('',#21293);
#3237=VERTEX_POINT('',#21300);
#3238=VERTEX_POINT('',#21302);
#3239=VERTEX_POINT('',#21309);
#3240=VERTEX_POINT('',#21311);
#3241=VERTEX_POINT('',#21318);
#3242=VERTEX_POINT('',#21320);
#3243=VERTEX_POINT('',#21325);
#3244=VERTEX_POINT('',#21328);
#3245=VERTEX_POINT('',#21333);
#3246=VERTEX_POINT('',#21335);
#3247=VERTEX_POINT('',#21342);
#3248=VERTEX_POINT('',#21344);
#3249=VERTEX_POINT('',#21351);
#3250=VERTEX_POINT('',#21353);
#3251=VERTEX_POINT('',#21360);
#3252=VERTEX_POINT('',#21362);
#3253=VERTEX_POINT('',#21369);
#3254=VERTEX_POINT('',#21371);
#3255=VERTEX_POINT('',#21380);
#3256=VERTEX_POINT('',#21393);
#3257=VERTEX_POINT('',#21394);
#3258=VERTEX_POINT('',#21396);
#3259=VERTEX_POINT('',#21414);
#3260=VERTEX_POINT('',#21432);
#3261=VERTEX_POINT('',#21446);
#3262=VERTEX_POINT('',#21459);
#3263=VERTEX_POINT('',#21460);
#3264=VERTEX_POINT('',#21462);
#3265=VERTEX_POINT('',#21480);
#3266=VERTEX_POINT('',#21498);
#3267=VERTEX_POINT('',#21512);
#3268=VERTEX_POINT('',#21525);
#3269=VERTEX_POINT('',#21526);
#3270=VERTEX_POINT('',#21528);
#3271=VERTEX_POINT('',#21546);
#3272=VERTEX_POINT('',#21564);
#3273=VERTEX_POINT('',#21578);
#3274=VERTEX_POINT('',#21591);
#3275=VERTEX_POINT('',#21592);
#3276=VERTEX_POINT('',#21594);
#3277=VERTEX_POINT('',#21595);
#3278=VERTEX_POINT('',#21615);
#3279=VERTEX_POINT('',#21616);
#3280=VERTEX_POINT('',#21636);
#3281=VERTEX_POINT('',#21650);
#3282=VERTEX_POINT('',#21663);
#3283=VERTEX_POINT('',#21664);
#3284=VERTEX_POINT('',#21666);
#3285=VERTEX_POINT('',#21684);
#3286=VERTEX_POINT('',#21702);
#3287=VERTEX_POINT('',#21716);
#3288=VERTEX_POINT('',#21729);
#3289=VERTEX_POINT('',#21730);
#3290=VERTEX_POINT('',#21732);
#3291=VERTEX_POINT('',#21750);
#3292=VERTEX_POINT('',#21768);
#3293=VERTEX_POINT('',#21782);
#3294=VERTEX_POINT('',#21795);
#3295=VERTEX_POINT('',#21796);
#3296=VERTEX_POINT('',#21798);
#3297=VERTEX_POINT('',#21816);
#3298=VERTEX_POINT('',#21834);
#3299=VERTEX_POINT('',#21848);
#3300=VERTEX_POINT('',#21861);
#3301=VERTEX_POINT('',#21862);
#3302=VERTEX_POINT('',#21864);
#3303=VERTEX_POINT('',#21882);
#3304=VERTEX_POINT('',#21900);
#3305=VERTEX_POINT('',#21902);
#3306=VERTEX_POINT('',#21910);
#3307=VERTEX_POINT('',#21926);
#3308=VERTEX_POINT('',#21929);
#3309=VERTEX_POINT('',#21931);
#3310=VERTEX_POINT('',#21951);
#3311=VERTEX_POINT('',#21952);
#3312=VERTEX_POINT('',#21977);
#3313=VERTEX_POINT('',#21980);
#3314=VERTEX_POINT('',#21984);
#3315=VERTEX_POINT('',#21988);
#3316=VERTEX_POINT('',#21992);
#3317=VERTEX_POINT('',#21998);
#3318=VERTEX_POINT('',#22001);
#3319=VERTEX_POINT('',#22005);
#3320=VERTEX_POINT('',#22009);
#3321=VERTEX_POINT('',#22015);
#3322=VERTEX_POINT('',#22017);
#3323=VERTEX_POINT('',#22020);
#3324=VERTEX_POINT('',#22024);
#3325=VERTEX_POINT('',#22027);
#3326=VERTEX_POINT('',#22031);
#3327=VERTEX_POINT('',#22034);
#3328=VERTEX_POINT('',#22038);
#3329=VERTEX_POINT('',#22042);
#3330=VERTEX_POINT('',#22046);
#3331=VERTEX_POINT('',#22049);
#3332=VERTEX_POINT('',#22053);
#3333=VERTEX_POINT('',#22056);
#3334=VERTEX_POINT('',#22060);
#3335=VERTEX_POINT('',#22063);
#3336=VERTEX_POINT('',#22067);
#3337=VERTEX_POINT('',#22074);
#3338=VERTEX_POINT('',#22076);
#3339=VERTEX_POINT('',#22080);
#3340=VERTEX_POINT('',#22083);
#3341=VERTEX_POINT('',#22089);
#3342=VERTEX_POINT('',#22090);
#3343=VERTEX_POINT('',#22092);
#3344=VERTEX_POINT('',#22103);
#3345=VERTEX_POINT('',#22113);
#3346=VERTEX_POINT('',#22114);
#3347=VERTEX_POINT('',#22161);
#3348=VERTEX_POINT('',#22162);
#3349=VERTEX_POINT('',#22215);
#3350=VERTEX_POINT('',#22216);
#3351=VERTEX_POINT('',#22263);
#3352=VERTEX_POINT('',#22264);
#3353=VERTEX_POINT('',#22314);
#3354=VERTEX_POINT('',#22315);
#3355=VERTEX_POINT('',#22317);
#3356=VERTEX_POINT('',#22328);
#3357=VERTEX_POINT('',#22340);
#3358=VERTEX_POINT('',#22341);
#3359=VERTEX_POINT('',#22364);
#3360=VERTEX_POINT('',#22365);
#3361=VERTEX_POINT('',#22389);
#3362=VERTEX_POINT('',#22390);
#3363=VERTEX_POINT('',#22414);
#3364=VERTEX_POINT('',#22500);
#3365=VERTEX_POINT('',#22502);
#3366=VERTEX_POINT('',#22748);
#3367=VERTEX_POINT('',#22844);
#3368=VERTEX_POINT('',#22847);
#3369=VERTEX_POINT('',#23097);
#3370=VERTEX_POINT('',#23098);
#3371=VERTEX_POINT('',#23102);
#3372=VERTEX_POINT('',#23103);
#3373=VERTEX_POINT('',#23105);
#3374=VERTEX_POINT('',#23107);
#3375=VERTEX_POINT('',#23111);
#3376=VERTEX_POINT('',#23113);
#3377=VERTEX_POINT('',#23117);
#3378=VERTEX_POINT('',#23119);
#3379=VERTEX_POINT('',#23123);
#3380=VERTEX_POINT('',#23125);
#3381=VERTEX_POINT('',#23129);
#3382=VERTEX_POINT('',#23131);
#3383=VERTEX_POINT('',#23139);
#3384=VERTEX_POINT('',#23146);
#3385=VERTEX_POINT('',#23152);
#3386=VERTEX_POINT('',#23154);
#3387=VERTEX_POINT('',#23158);
#3388=VERTEX_POINT('',#23160);
#3389=VERTEX_POINT('',#23164);
#3390=VERTEX_POINT('',#23165);
#3391=VERTEX_POINT('',#23167);
#3392=VERTEX_POINT('',#23169);
#3393=VERTEX_POINT('',#23173);
#3394=VERTEX_POINT('',#23175);
#3395=VERTEX_POINT('',#23177);
#3396=VERTEX_POINT('',#23179);
#3397=VERTEX_POINT('',#23181);
#3398=VERTEX_POINT('',#23183);
#3399=VERTEX_POINT('',#23187);
#3400=VERTEX_POINT('',#23189);
#3401=VERTEX_POINT('',#23193);
#3402=VERTEX_POINT('',#23199);
#3403=VERTEX_POINT('',#23203);
#3404=VERTEX_POINT('',#23205);
#3405=EDGE_CURVE('',#2702,#2702,#2359,.T.);
#3406=EDGE_CURVE('',#2702,#2703,#1841,.T.);
#3407=EDGE_CURVE('',#2703,#2703,#2360,.T.);
#3408=EDGE_CURVE('',#2704,#2704,#2361,.T.);
#3409=EDGE_CURVE('',#2704,#2705,#1842,.T.);
#3410=EDGE_CURVE('',#2705,#2705,#2362,.T.);
#3411=EDGE_CURVE('',#2706,#2706,#2363,.T.);
#3412=EDGE_CURVE('',#2706,#2707,#1843,.T.);
#3413=EDGE_CURVE('',#2707,#2707,#2364,.T.);
#3414=EDGE_CURVE('',#2708,#2708,#2365,.T.);
#3415=EDGE_CURVE('',#2708,#2709,#1844,.T.);
#3416=EDGE_CURVE('',#2709,#2709,#2366,.T.);
#3417=EDGE_CURVE('',#2710,#2710,#2367,.T.);
#3418=EDGE_CURVE('',#2710,#2711,#1845,.T.);
#3419=EDGE_CURVE('',#2711,#2711,#2368,.T.);
#3420=EDGE_CURVE('',#2712,#2712,#2369,.T.);
#3421=EDGE_CURVE('',#2712,#2713,#1846,.T.);
#3422=EDGE_CURVE('',#2713,#2713,#2370,.T.);
#3423=EDGE_CURVE('',#2714,#2714,#2371,.T.);
#3424=EDGE_CURVE('',#2714,#2715,#1847,.T.);
#3425=EDGE_CURVE('',#2715,#2715,#2372,.T.);
#3426=EDGE_CURVE('',#2716,#2716,#2373,.T.);
#3427=EDGE_CURVE('',#2716,#2717,#1848,.T.);
#3428=EDGE_CURVE('',#2717,#2717,#2374,.T.);
#3429=EDGE_CURVE('',#2718,#2718,#2375,.T.);
#3430=EDGE_CURVE('',#2718,#2719,#1849,.T.);
#3431=EDGE_CURVE('',#2719,#2719,#2376,.T.);
#3432=EDGE_CURVE('',#2720,#2720,#2377,.T.);
#3433=EDGE_CURVE('',#2720,#2721,#1850,.T.);
#3434=EDGE_CURVE('',#2721,#2721,#2378,.T.);
#3435=EDGE_CURVE('',#2722,#2722,#2379,.T.);
#3436=EDGE_CURVE('',#2722,#2723,#1851,.T.);
#3437=EDGE_CURVE('',#2723,#2723,#2380,.T.);
#3438=EDGE_CURVE('',#2724,#2724,#2381,.T.);
#3439=EDGE_CURVE('',#2724,#2725,#1852,.T.);
#3440=EDGE_CURVE('',#2725,#2725,#2382,.T.);
#3441=EDGE_CURVE('',#2726,#2726,#2383,.T.);
#3442=EDGE_CURVE('',#2726,#2727,#1853,.T.);
#3443=EDGE_CURVE('',#2727,#2727,#2384,.T.);
#3444=EDGE_CURVE('',#2728,#2729,#2385,.T.);
#3445=EDGE_CURVE('',#2729,#2730,#2386,.T.);
#3446=EDGE_CURVE('',#2730,#2730,#2387,.T.);
#3447=EDGE_CURVE('',#2729,#2728,#2388,.T.);
#3448=EDGE_CURVE('',#2728,#2731,#1854,.T.);
#3449=EDGE_CURVE('',#2732,#2731,#2389,.T.);
#3450=EDGE_CURVE('',#2731,#2732,#2390,.T.);
#3451=EDGE_CURVE('',#2733,#2734,#1855,.T.);
#3452=EDGE_CURVE('',#2735,#2733,#2391,.T.);
#3453=EDGE_CURVE('',#2736,#2735,#1856,.T.);
#3454=EDGE_CURVE('',#2737,#2736,#2392,.T.);
#3455=EDGE_CURVE('',#2738,#2737,#1857,.T.);
#3456=EDGE_CURVE('',#2739,#2738,#2393,.T.);
#3457=EDGE_CURVE('',#2740,#2739,#1858,.T.);
#3458=EDGE_CURVE('',#2734,#2740,#2394,.T.);
#3459=EDGE_CURVE('',#2732,#2741,#1859,.T.);
#3460=EDGE_CURVE('',#2741,#2741,#2395,.T.);
#3461=EDGE_CURVE('',#2742,#2733,#1860,.T.);
#3462=EDGE_CURVE('',#2734,#2743,#1861,.T.);
#3463=EDGE_CURVE('',#2743,#2742,#1862,.T.);
#3464=EDGE_CURVE('',#2742,#2744,#2396,.T.);
#3465=EDGE_CURVE('',#2744,#2735,#1863,.T.);
#3466=EDGE_CURVE('',#2745,#2736,#1864,.T.);
#3467=EDGE_CURVE('',#2744,#2745,#1865,.T.);
#3468=EDGE_CURVE('',#2745,#2746,#2397,.T.);
#3469=EDGE_CURVE('',#2746,#2737,#1866,.T.);
#3470=EDGE_CURVE('',#2746,#2747,#1867,.T.);
#3471=EDGE_CURVE('',#2747,#2738,#1868,.T.);
#3472=EDGE_CURVE('',#2747,#2748,#2398,.T.);
#3473=EDGE_CURVE('',#2748,#2739,#1869,.T.);
#3474=EDGE_CURVE('',#2748,#2749,#1870,.T.);
#3475=EDGE_CURVE('',#2749,#2740,#1871,.T.);
#3476=EDGE_CURVE('',#2749,#2743,#2399,.T.);
#3477=EDGE_CURVE('',#2745,#2750,#1872,.T.);
#3478=EDGE_CURVE('',#2751,#2750,#2400,.T.);
#3479=EDGE_CURVE('',#2751,#2746,#1873,.T.);
#3480=EDGE_CURVE('',#2752,#2744,#1874,.T.);
#3481=EDGE_CURVE('',#2750,#2752,#1875,.T.);
#3482=EDGE_CURVE('',#2742,#2753,#1876,.T.);
#3483=EDGE_CURVE('',#2752,#2753,#2401,.T.);
#3484=EDGE_CURVE('',#2754,#2743,#1877,.T.);
#3485=EDGE_CURVE('',#2753,#2754,#1878,.T.);
#3486=EDGE_CURVE('',#2755,#2751,#1879,.T.);
#3487=EDGE_CURVE('',#2750,#2756,#1880,.T.);
#3488=EDGE_CURVE('',#2756,#2755,#2402,.T.);
#3489=EDGE_CURVE('',#2757,#2758,#1881,.T.);
#3490=EDGE_CURVE('',#2758,#2751,#1882,.T.);
#3491=EDGE_CURVE('',#2755,#2757,#1883,.T.);
#3492=EDGE_CURVE('',#2759,#2760,#1884,.T.);
#3493=EDGE_CURVE('',#2760,#2758,#2403,.T.);
#3494=EDGE_CURVE('',#2757,#2759,#2404,.T.);
#3495=EDGE_CURVE('',#2759,#2761,#1885,.T.);
#3496=EDGE_CURVE('',#2761,#2762,#1886,.T.);
#3497=EDGE_CURVE('',#2762,#2760,#1887,.T.);
#3498=EDGE_CURVE('',#2763,#2754,#1888,.T.);
#3499=EDGE_CURVE('',#2754,#2762,#2405,.T.);
#3500=EDGE_CURVE('',#2761,#2763,#2406,.T.);
#3501=EDGE_CURVE('',#2763,#2764,#1889,.T.);
#3502=EDGE_CURVE('',#2764,#2753,#1890,.T.);
#3503=EDGE_CURVE('',#2765,#2752,#1891,.T.);
#3504=EDGE_CURVE('',#2764,#2765,#2407,.T.);
#3505=EDGE_CURVE('',#2765,#2756,#1892,.T.);
#3506=EDGE_CURVE('',#2766,#2767,#2408,.T.);
#3507=EDGE_CURVE('',#2768,#2766,#1893,.T.);
#3508=EDGE_CURVE('',#2769,#2768,#2409,.T.);
#3509=EDGE_CURVE('',#2770,#2769,#1894,.T.);
#3510=EDGE_CURVE('',#2771,#2770,#2410,.T.);
#3511=EDGE_CURVE('',#2772,#2771,#1895,.T.);
#3512=EDGE_CURVE('',#2773,#2772,#2411,.T.);
#3513=EDGE_CURVE('',#2767,#2773,#1896,.T.);
#3514=EDGE_CURVE('',#2767,#2774,#1897,.T.);
#3515=EDGE_CURVE('',#2774,#2775,#2412,.T.);
#3516=EDGE_CURVE('',#2775,#2766,#1898,.T.);
#3517=EDGE_CURVE('',#2773,#2776,#1899,.T.);
#3518=EDGE_CURVE('',#2776,#2774,#1900,.T.);
#3519=EDGE_CURVE('',#2772,#2777,#1901,.T.);
#3520=EDGE_CURVE('',#2777,#2776,#2413,.T.);
#3521=EDGE_CURVE('',#2771,#2778,#1902,.T.);
#3522=EDGE_CURVE('',#2778,#2777,#1903,.T.);
#3523=EDGE_CURVE('',#2770,#2779,#1904,.T.);
#3524=EDGE_CURVE('',#2779,#2778,#2414,.T.);
#3525=EDGE_CURVE('',#2769,#2780,#1905,.T.);
#3526=EDGE_CURVE('',#2780,#2779,#1906,.T.);
#3527=EDGE_CURVE('',#2768,#2781,#1907,.T.);
#3528=EDGE_CURVE('',#2781,#2780,#2415,.T.);
#3529=EDGE_CURVE('',#2775,#2781,#1908,.T.);
#3530=EDGE_CURVE('',#2782,#2780,#1909,.T.);
#3531=EDGE_CURVE('',#2783,#2782,#1910,.T.);
#3532=EDGE_CURVE('',#2779,#2783,#1911,.T.);
#3533=EDGE_CURVE('',#2781,#2784,#1912,.T.);
#3534=EDGE_CURVE('',#2782,#2784,#2416,.T.);
#3535=EDGE_CURVE('',#2785,#2775,#1913,.T.);
#3536=EDGE_CURVE('',#2784,#2785,#1914,.T.);
#3537=EDGE_CURVE('',#2774,#2786,#1915,.T.);
#3538=EDGE_CURVE('',#2785,#2786,#2417,.T.);
#3539=EDGE_CURVE('',#2787,#2786,#1916,.T.);
#3540=EDGE_CURVE('',#2787,#2788,#2418,.T.);
#3541=EDGE_CURVE('',#2789,#2788,#1917,.T.);
#3542=EDGE_CURVE('',#2789,#2783,#2419,.T.);
#3543=EDGE_CURVE('',#2787,#2776,#1918,.T.);
#3544=EDGE_CURVE('',#2777,#2788,#1919,.T.);
#3545=EDGE_CURVE('',#2789,#2778,#1920,.T.);
#3546=EDGE_CURVE('',#2747,#2758,#1921,.T.);
#3547=EDGE_CURVE('',#2760,#2748,#1922,.T.);
#3548=EDGE_CURVE('',#2749,#2762,#1923,.T.);
#3549=EDGE_CURVE('',#2790,#2791,#1924,.T.);
#3550=EDGE_CURVE('',#2790,#2792,#335,.T.);
#3551=EDGE_CURVE('',#2792,#2793,#2420,.T.);
#3552=EDGE_CURVE('',#2793,#2791,#336,.T.);
#3553=EDGE_CURVE('',#2794,#2795,#337,.T.);
#3554=EDGE_CURVE('',#2796,#2794,#338,.T.);
#3555=EDGE_CURVE('',#2795,#2796,#339,.T.);
#3556=EDGE_CURVE('',#2795,#2797,#1925,.T.);
#3557=EDGE_CURVE('',#2797,#2797,#2421,.T.);
#3558=EDGE_CURVE('',#2797,#2798,#1926,.T.);
#3559=EDGE_CURVE('',#2799,#2798,#340,.T.);
#3560=EDGE_CURVE('',#2800,#2799,#341,.T.);
#3561=EDGE_CURVE('',#2798,#2800,#342,.T.);
#3562=EDGE_CURVE('',#2801,#2802,#343,.T.);
#3563=EDGE_CURVE('',#2801,#2803,#1927,.T.);
#3564=EDGE_CURVE('',#2803,#2803,#2422,.T.);
#3565=EDGE_CURVE('',#2802,#2801,#344,.T.);
#3566=EDGE_CURVE('',#2803,#2804,#1928,.T.);
#3567=EDGE_CURVE('',#2805,#2804,#345,.T.);
#3568=EDGE_CURVE('',#2804,#2805,#346,.T.);
#3569=EDGE_CURVE('',#2806,#2806,#2423,.T.);
#3570=EDGE_CURVE('',#2806,#2807,#1929,.T.);
#3571=EDGE_CURVE('',#2807,#2808,#2424,.T.);
#3572=EDGE_CURVE('',#2808,#2807,#2425,.T.);
#3573=EDGE_CURVE('',#2809,#2810,#2426,.T.);
#3574=EDGE_CURVE('',#2810,#2809,#2427,.T.);
#3575=EDGE_CURVE('',#2810,#2799,#1930,.T.);
#3576=EDGE_CURVE('',#2800,#2808,#1931,.T.);
#3577=EDGE_CURVE('',#2811,#2812,#2428,.T.);
#3578=EDGE_CURVE('',#2811,#2813,#175,.T.);
#3579=EDGE_CURVE('',#2813,#2814,#176,.T.);
#3580=EDGE_CURVE('',#2815,#2814,#2429,.T.);
#3581=EDGE_CURVE('',#2815,#2816,#177,.T.);
#3582=EDGE_CURVE('',#2816,#2817,#178,.T.);
#3583=EDGE_CURVE('',#2818,#2817,#2430,.T.);
#3584=EDGE_CURVE('',#2818,#2819,#179,.T.);
#3585=EDGE_CURVE('',#2819,#2820,#180,.T.);
#3586=EDGE_CURVE('',#2821,#2820,#2431,.T.);
#3587=EDGE_CURVE('',#2821,#2822,#181,.T.);
#3588=EDGE_CURVE('',#2822,#2823,#182,.T.);
#3589=EDGE_CURVE('',#2824,#2823,#2432,.T.);
#3590=EDGE_CURVE('',#2824,#2825,#183,.T.);
#3591=EDGE_CURVE('',#2825,#2826,#184,.T.);
#3592=EDGE_CURVE('',#2827,#2826,#2433,.T.);
#3593=EDGE_CURVE('',#2827,#2828,#185,.T.);
#3594=EDGE_CURVE('',#2828,#2829,#186,.T.);
#3595=EDGE_CURVE('',#2830,#2829,#2434,.T.);
#3596=EDGE_CURVE('',#2830,#2831,#187,.T.);
#3597=EDGE_CURVE('',#2831,#2832,#188,.T.);
#3598=EDGE_CURVE('',#2833,#2832,#2435,.T.);
#3599=EDGE_CURVE('',#2833,#2834,#189,.T.);
#3600=EDGE_CURVE('',#2834,#2835,#190,.T.);
#3601=EDGE_CURVE('',#2836,#2835,#2436,.T.);
#3602=EDGE_CURVE('',#2836,#2837,#191,.T.);
#3603=EDGE_CURVE('',#2837,#2793,#192,.T.);
#3604=EDGE_CURVE('',#2792,#2838,#193,.T.);
#3605=EDGE_CURVE('',#2838,#2839,#194,.T.);
#3606=EDGE_CURVE('',#2840,#2839,#2437,.T.);
#3607=EDGE_CURVE('',#2840,#2841,#195,.T.);
#3608=EDGE_CURVE('',#2841,#2842,#196,.T.);
#3609=EDGE_CURVE('',#2843,#2842,#2438,.T.);
#3610=EDGE_CURVE('',#2843,#2844,#197,.T.);
#3611=EDGE_CURVE('',#2844,#2845,#198,.T.);
#3612=EDGE_CURVE('',#2846,#2845,#2439,.T.);
#3613=EDGE_CURVE('',#2846,#2847,#199,.T.);
#3614=EDGE_CURVE('',#2847,#2848,#200,.T.);
#3615=EDGE_CURVE('',#2849,#2848,#2440,.T.);
#3616=EDGE_CURVE('',#2849,#2850,#201,.T.);
#3617=EDGE_CURVE('',#2850,#2851,#202,.T.);
#3618=EDGE_CURVE('',#2852,#2851,#2441,.T.);
#3619=EDGE_CURVE('',#2852,#2853,#203,.T.);
#3620=EDGE_CURVE('',#2853,#2854,#204,.T.);
#3621=EDGE_CURVE('',#2855,#2854,#2442,.T.);
#3622=EDGE_CURVE('',#2855,#2856,#205,.T.);
#3623=EDGE_CURVE('',#2856,#2857,#206,.T.);
#3624=EDGE_CURVE('',#2858,#2857,#2443,.T.);
#3625=EDGE_CURVE('',#2858,#2859,#207,.T.);
#3626=EDGE_CURVE('',#2859,#2860,#208,.T.);
#3627=EDGE_CURVE('',#2861,#2860,#2444,.T.);
#3628=EDGE_CURVE('',#2861,#2862,#209,.T.);
#3629=EDGE_CURVE('',#2862,#2863,#210,.T.);
#3630=EDGE_CURVE('',#2864,#2863,#2445,.T.);
#3631=EDGE_CURVE('',#2864,#2865,#211,.T.);
#3632=EDGE_CURVE('',#2865,#2866,#212,.T.);
#3633=EDGE_CURVE('',#2867,#2866,#2446,.T.);
#3634=EDGE_CURVE('',#2867,#2868,#213,.T.);
#3635=EDGE_CURVE('',#2868,#2812,#214,.T.);
#3636=EDGE_CURVE('',#2809,#2869,#1932,.T.);
#3637=EDGE_CURVE('',#2869,#2869,#2447,.T.);
#3638=EDGE_CURVE('',#2870,#2870,#2448,.T.);
#3639=EDGE_CURVE('',#2870,#2871,#1933,.T.);
#3640=EDGE_CURVE('',#2871,#2872,#2449,.T.);
#3641=EDGE_CURVE('',#2872,#2871,#2450,.T.);
#3642=EDGE_CURVE('',#2872,#2796,#1934,.T.);
#3643=EDGE_CURVE('',#2794,#2873,#1935,.T.);
#3644=EDGE_CURVE('',#2873,#2873,#2451,.T.);
#3645=EDGE_CURVE('',#2874,#2875,#347,.T.);
#3646=EDGE_CURVE('',#2876,#2874,#348,.T.);
#3647=EDGE_CURVE('',#2875,#2876,#2452,.T.);
#3648=EDGE_CURVE('',#2877,#2878,#349,.T.);
#3649=EDGE_CURVE('',#2879,#2877,#350,.T.);
#3650=EDGE_CURVE('',#2878,#2879,#2453,.T.);
#3651=EDGE_CURVE('',#2880,#2881,#351,.T.);
#3652=EDGE_CURVE('',#2882,#2880,#352,.T.);
#3653=EDGE_CURVE('',#2881,#2882,#2454,.T.);
#3654=EDGE_CURVE('',#2883,#2884,#353,.T.);
#3655=EDGE_CURVE('',#2885,#2883,#354,.T.);
#3656=EDGE_CURVE('',#2884,#2885,#2455,.T.);
#3657=EDGE_CURVE('',#2886,#2887,#355,.T.);
#3658=EDGE_CURVE('',#2888,#2886,#356,.T.);
#3659=EDGE_CURVE('',#2887,#2888,#2456,.T.);
#3660=EDGE_CURVE('',#2889,#2890,#357,.T.);
#3661=EDGE_CURVE('',#2891,#2889,#358,.T.);
#3662=EDGE_CURVE('',#2890,#2891,#2457,.T.);
#3663=EDGE_CURVE('',#2892,#2893,#359,.T.);
#3664=EDGE_CURVE('',#2894,#2892,#360,.T.);
#3665=EDGE_CURVE('',#2893,#2894,#2458,.T.);
#3666=EDGE_CURVE('',#2895,#2896,#361,.T.);
#3667=EDGE_CURVE('',#2897,#2895,#362,.T.);
#3668=EDGE_CURVE('',#2896,#2897,#2459,.T.);
#3669=EDGE_CURVE('',#2898,#2899,#363,.T.);
#3670=EDGE_CURVE('',#2900,#2898,#364,.T.);
#3671=EDGE_CURVE('',#2899,#2900,#2460,.T.);
#3672=EDGE_CURVE('',#2901,#2902,#365,.T.);
#3673=EDGE_CURVE('',#2903,#2901,#366,.T.);
#3674=EDGE_CURVE('',#2902,#2903,#2461,.T.);
#3675=EDGE_CURVE('',#2904,#2905,#367,.T.);
#3676=EDGE_CURVE('',#2906,#2904,#368,.T.);
#3677=EDGE_CURVE('',#2905,#2906,#2462,.T.);
#3678=EDGE_CURVE('',#2907,#2908,#369,.T.);
#3679=EDGE_CURVE('',#2909,#2907,#370,.T.);
#3680=EDGE_CURVE('',#2908,#2909,#2463,.T.);
#3681=EDGE_CURVE('',#2910,#2911,#371,.T.);
#3682=EDGE_CURVE('',#2912,#2910,#372,.T.);
#3683=EDGE_CURVE('',#2911,#2912,#2464,.T.);
#3684=EDGE_CURVE('',#2913,#2914,#373,.T.);
#3685=EDGE_CURVE('',#2915,#2913,#374,.T.);
#3686=EDGE_CURVE('',#2914,#2915,#2465,.T.);
#3687=EDGE_CURVE('',#2916,#2917,#375,.T.);
#3688=EDGE_CURVE('',#2918,#2916,#376,.T.);
#3689=EDGE_CURVE('',#2917,#2918,#2466,.T.);
#3690=EDGE_CURVE('',#2919,#2920,#377,.T.);
#3691=EDGE_CURVE('',#2921,#2919,#378,.T.);
#3692=EDGE_CURVE('',#2920,#2921,#2467,.T.);
#3693=EDGE_CURVE('',#2922,#2923,#379,.T.);
#3694=EDGE_CURVE('',#2924,#2922,#380,.T.);
#3695=EDGE_CURVE('',#2923,#2924,#2468,.T.);
#3696=EDGE_CURVE('',#2925,#2926,#381,.T.);
#3697=EDGE_CURVE('',#2927,#2925,#382,.T.);
#3698=EDGE_CURVE('',#2926,#2927,#2469,.T.);
#3699=EDGE_CURVE('',#2928,#2929,#383,.T.);
#3700=EDGE_CURVE('',#2930,#2928,#384,.T.);
#3701=EDGE_CURVE('',#2929,#2930,#2470,.T.);
#3702=EDGE_CURVE('',#2931,#2931,#2471,.T.);
#3703=EDGE_CURVE('',#2931,#2932,#1936,.T.);
#3704=EDGE_CURVE('',#2932,#2932,#2472,.T.);
#3705=EDGE_CURVE('',#2932,#2933,#1937,.T.);
#3706=EDGE_CURVE('',#2933,#2933,#2473,.T.);
#3707=EDGE_CURVE('',#2934,#2935,#385,.T.);
#3708=EDGE_CURVE('',#2936,#2934,#386,.T.);
#3709=EDGE_CURVE('',#2935,#2936,#2474,.T.);
#3710=EDGE_CURVE('',#2868,#2934,#1938,.T.);
#3711=EDGE_CURVE('',#2937,#2867,#387,.T.);
#3712=EDGE_CURVE('',#2937,#2936,#215,.T.);
#3713=EDGE_CURVE('',#2813,#2928,#1939,.T.);
#3714=EDGE_CURVE('',#2938,#2811,#388,.T.);
#3715=EDGE_CURVE('',#2938,#2930,#216,.T.);
#3716=EDGE_CURVE('',#2816,#2925,#1940,.T.);
#3717=EDGE_CURVE('',#2939,#2815,#389,.T.);
#3718=EDGE_CURVE('',#2939,#2927,#217,.T.);
#3719=EDGE_CURVE('',#2819,#2922,#1941,.T.);
#3720=EDGE_CURVE('',#2940,#2818,#390,.T.);
#3721=EDGE_CURVE('',#2940,#2924,#218,.T.);
#3722=EDGE_CURVE('',#2822,#2919,#1942,.T.);
#3723=EDGE_CURVE('',#2941,#2821,#391,.T.);
#3724=EDGE_CURVE('',#2941,#2921,#219,.T.);
#3725=EDGE_CURVE('',#2825,#2916,#1943,.T.);
#3726=EDGE_CURVE('',#2942,#2824,#392,.T.);
#3727=EDGE_CURVE('',#2942,#2918,#220,.T.);
#3728=EDGE_CURVE('',#2828,#2913,#1944,.T.);
#3729=EDGE_CURVE('',#2943,#2827,#393,.T.);
#3730=EDGE_CURVE('',#2943,#2915,#221,.T.);
#3731=EDGE_CURVE('',#2831,#2910,#1945,.T.);
#3732=EDGE_CURVE('',#2944,#2830,#394,.T.);
#3733=EDGE_CURVE('',#2944,#2912,#222,.T.);
#3734=EDGE_CURVE('',#2834,#2907,#1946,.T.);
#3735=EDGE_CURVE('',#2945,#2833,#395,.T.);
#3736=EDGE_CURVE('',#2945,#2909,#223,.T.);
#3737=EDGE_CURVE('',#2837,#2904,#1947,.T.);
#3738=EDGE_CURVE('',#2946,#2836,#396,.T.);
#3739=EDGE_CURVE('',#2946,#2906,#224,.T.);
#3740=EDGE_CURVE('',#2838,#2901,#1948,.T.);
#3741=EDGE_CURVE('',#2947,#2790,#397,.T.);
#3742=EDGE_CURVE('',#2947,#2903,#225,.T.);
#3743=EDGE_CURVE('',#2841,#2898,#1949,.T.);
#3744=EDGE_CURVE('',#2948,#2840,#398,.T.);
#3745=EDGE_CURVE('',#2948,#2900,#226,.T.);
#3746=EDGE_CURVE('',#2844,#2895,#1950,.T.);
#3747=EDGE_CURVE('',#2949,#2843,#399,.T.);
#3748=EDGE_CURVE('',#2949,#2897,#227,.T.);
#3749=EDGE_CURVE('',#2847,#2892,#1951,.T.);
#3750=EDGE_CURVE('',#2950,#2846,#400,.T.);
#3751=EDGE_CURVE('',#2950,#2894,#228,.T.);
#3752=EDGE_CURVE('',#2850,#2889,#1952,.T.);
#3753=EDGE_CURVE('',#2951,#2849,#401,.T.);
#3754=EDGE_CURVE('',#2951,#2891,#229,.T.);
#3755=EDGE_CURVE('',#2853,#2886,#1953,.T.);
#3756=EDGE_CURVE('',#2952,#2852,#402,.T.);
#3757=EDGE_CURVE('',#2952,#2888,#230,.T.);
#3758=EDGE_CURVE('',#2856,#2883,#1954,.T.);
#3759=EDGE_CURVE('',#2953,#2855,#403,.T.);
#3760=EDGE_CURVE('',#2953,#2885,#231,.T.);
#3761=EDGE_CURVE('',#2859,#2880,#1955,.T.);
#3762=EDGE_CURVE('',#2954,#2858,#404,.T.);
#3763=EDGE_CURVE('',#2954,#2882,#232,.T.);
#3764=EDGE_CURVE('',#2862,#2877,#1956,.T.);
#3765=EDGE_CURVE('',#2955,#2861,#405,.T.);
#3766=EDGE_CURVE('',#2955,#2879,#233,.T.);
#3767=EDGE_CURVE('',#2865,#2874,#1957,.T.);
#3768=EDGE_CURVE('',#2956,#2864,#406,.T.);
#3769=EDGE_CURVE('',#2956,#2876,#234,.T.);
#3770=EDGE_CURVE('',#2935,#2957,#235,.T.);
#3771=EDGE_CURVE('',#2812,#2957,#407,.T.);
#3772=EDGE_CURVE('',#2957,#2937,#2475,.T.);
#3773=EDGE_CURVE('',#2931,#2958,#1958,.T.);
#3774=EDGE_CURVE('',#2958,#2947,#2476,.T.);
#3775=EDGE_CURVE('',#2791,#2959,#408,.T.);
#3776=EDGE_CURVE('',#2959,#2946,#2477,.T.);
#3777=EDGE_CURVE('',#2835,#2960,#409,.T.);
#3778=EDGE_CURVE('',#2960,#2945,#2478,.T.);
#3779=EDGE_CURVE('',#2832,#2961,#410,.T.);
#3780=EDGE_CURVE('',#2961,#2944,#2479,.T.);
#3781=EDGE_CURVE('',#2829,#2962,#411,.T.);
#3782=EDGE_CURVE('',#2962,#2943,#2480,.T.);
#3783=EDGE_CURVE('',#2826,#2963,#412,.T.);
#3784=EDGE_CURVE('',#2963,#2942,#2481,.T.);
#3785=EDGE_CURVE('',#2823,#2964,#413,.T.);
#3786=EDGE_CURVE('',#2964,#2941,#2482,.T.);
#3787=EDGE_CURVE('',#2820,#2965,#414,.T.);
#3788=EDGE_CURVE('',#2965,#2940,#2483,.T.);
#3789=EDGE_CURVE('',#2817,#2966,#415,.T.);
#3790=EDGE_CURVE('',#2966,#2939,#2484,.T.);
#3791=EDGE_CURVE('',#2814,#2967,#416,.T.);
#3792=EDGE_CURVE('',#2967,#2938,#2485,.T.);
#3793=EDGE_CURVE('',#2866,#2968,#417,.T.);
#3794=EDGE_CURVE('',#2968,#2956,#2486,.T.);
#3795=EDGE_CURVE('',#2863,#2969,#418,.T.);
#3796=EDGE_CURVE('',#2969,#2955,#2487,.T.);
#3797=EDGE_CURVE('',#2860,#2970,#419,.T.);
#3798=EDGE_CURVE('',#2970,#2954,#2488,.T.);
#3799=EDGE_CURVE('',#2857,#2971,#420,.T.);
#3800=EDGE_CURVE('',#2971,#2953,#2489,.T.);
#3801=EDGE_CURVE('',#2854,#2972,#421,.T.);
#3802=EDGE_CURVE('',#2972,#2952,#2490,.T.);
#3803=EDGE_CURVE('',#2851,#2973,#422,.T.);
#3804=EDGE_CURVE('',#2973,#2951,#2491,.T.);
#3805=EDGE_CURVE('',#2848,#2974,#423,.T.);
#3806=EDGE_CURVE('',#2974,#2950,#2492,.T.);
#3807=EDGE_CURVE('',#2845,#2975,#424,.T.);
#3808=EDGE_CURVE('',#2975,#2949,#2493,.T.);
#3809=EDGE_CURVE('',#2842,#2976,#425,.T.);
#3810=EDGE_CURVE('',#2976,#2948,#2494,.T.);
#3811=EDGE_CURVE('',#2839,#2977,#426,.T.);
#3812=EDGE_CURVE('',#2977,#2958,#2495,.T.);
#3813=EDGE_CURVE('',#2929,#2967,#236,.T.);
#3814=EDGE_CURVE('',#2926,#2966,#237,.T.);
#3815=EDGE_CURVE('',#2923,#2965,#238,.T.);
#3816=EDGE_CURVE('',#2920,#2964,#239,.T.);
#3817=EDGE_CURVE('',#2917,#2963,#240,.T.);
#3818=EDGE_CURVE('',#2914,#2962,#241,.T.);
#3819=EDGE_CURVE('',#2911,#2961,#242,.T.);
#3820=EDGE_CURVE('',#2908,#2960,#243,.T.);
#3821=EDGE_CURVE('',#2905,#2959,#244,.T.);
#3822=EDGE_CURVE('',#2902,#2977,#245,.T.);
#3823=EDGE_CURVE('',#2899,#2976,#246,.T.);
#3824=EDGE_CURVE('',#2896,#2975,#247,.T.);
#3825=EDGE_CURVE('',#2893,#2974,#248,.T.);
#3826=EDGE_CURVE('',#2890,#2973,#249,.T.);
#3827=EDGE_CURVE('',#2887,#2972,#250,.T.);
#3828=EDGE_CURVE('',#2884,#2971,#251,.T.);
#3829=EDGE_CURVE('',#2881,#2970,#252,.T.);
#3830=EDGE_CURVE('',#2878,#2969,#253,.T.);
#3831=EDGE_CURVE('',#2875,#2968,#254,.T.);
#3832=EDGE_CURVE('',#2978,#2979,#427,.T.);
#3833=EDGE_CURVE('',#2980,#2978,#428,.T.);
#3834=EDGE_CURVE('',#2979,#2980,#429,.T.);
#3835=EDGE_CURVE('',#2979,#2981,#1959,.T.);
#3836=EDGE_CURVE('',#2981,#2981,#2496,.T.);
#3837=EDGE_CURVE('',#2981,#2982,#1960,.T.);
#3838=EDGE_CURVE('',#2983,#2982,#430,.T.);
#3839=EDGE_CURVE('',#2984,#2983,#431,.T.);
#3840=EDGE_CURVE('',#2982,#2984,#432,.T.);
#3841=EDGE_CURVE('',#2985,#2986,#433,.T.);
#3842=EDGE_CURVE('',#2985,#2987,#1961,.T.);
#3843=EDGE_CURVE('',#2987,#2987,#2497,.T.);
#3844=EDGE_CURVE('',#2986,#2985,#434,.T.);
#3845=EDGE_CURVE('',#2987,#2988,#1962,.T.);
#3846=EDGE_CURVE('',#2989,#2988,#435,.T.);
#3847=EDGE_CURVE('',#2988,#2989,#436,.T.);
#3848=EDGE_CURVE('',#2990,#2990,#2498,.T.);
#3849=EDGE_CURVE('',#2990,#2991,#1963,.T.);
#3850=EDGE_CURVE('',#2991,#2992,#2499,.T.);
#3851=EDGE_CURVE('',#2992,#2991,#2500,.T.);
#3852=EDGE_CURVE('',#2993,#2994,#2501,.T.);
#3853=EDGE_CURVE('',#2994,#2993,#2502,.T.);
#3854=EDGE_CURVE('',#2994,#2983,#1964,.T.);
#3855=EDGE_CURVE('',#2984,#2992,#1965,.T.);
#3856=EDGE_CURVE('',#2995,#2996,#2503,.T.);
#3857=EDGE_CURVE('',#2995,#2997,#255,.T.);
#3858=EDGE_CURVE('',#2997,#2998,#256,.T.);
#3859=EDGE_CURVE('',#2999,#2998,#2504,.T.);
#3860=EDGE_CURVE('',#2999,#3000,#257,.T.);
#3861=EDGE_CURVE('',#3000,#3001,#258,.T.);
#3862=EDGE_CURVE('',#3002,#3001,#2505,.T.);
#3863=EDGE_CURVE('',#3002,#3003,#259,.T.);
#3864=EDGE_CURVE('',#3003,#3004,#260,.T.);
#3865=EDGE_CURVE('',#3005,#3004,#2506,.T.);
#3866=EDGE_CURVE('',#3005,#3006,#261,.T.);
#3867=EDGE_CURVE('',#3006,#3007,#262,.T.);
#3868=EDGE_CURVE('',#3008,#3007,#2507,.T.);
#3869=EDGE_CURVE('',#3008,#3009,#263,.T.);
#3870=EDGE_CURVE('',#3009,#3010,#264,.T.);
#3871=EDGE_CURVE('',#3011,#3010,#2508,.T.);
#3872=EDGE_CURVE('',#3011,#3012,#265,.T.);
#3873=EDGE_CURVE('',#3012,#3013,#266,.T.);
#3874=EDGE_CURVE('',#3014,#3013,#2509,.T.);
#3875=EDGE_CURVE('',#3014,#3015,#267,.T.);
#3876=EDGE_CURVE('',#3015,#3016,#268,.T.);
#3877=EDGE_CURVE('',#3017,#3016,#2510,.T.);
#3878=EDGE_CURVE('',#3017,#3018,#269,.T.);
#3879=EDGE_CURVE('',#3018,#3019,#270,.T.);
#3880=EDGE_CURVE('',#3020,#3019,#2511,.T.);
#3881=EDGE_CURVE('',#3020,#3021,#271,.T.);
#3882=EDGE_CURVE('',#3021,#3022,#272,.T.);
#3883=EDGE_CURVE('',#3023,#3022,#2512,.T.);
#3884=EDGE_CURVE('',#3023,#3024,#273,.T.);
#3885=EDGE_CURVE('',#3024,#3025,#274,.T.);
#3886=EDGE_CURVE('',#3026,#3025,#2513,.T.);
#3887=EDGE_CURVE('',#3026,#3027,#275,.T.);
#3888=EDGE_CURVE('',#3027,#3028,#276,.T.);
#3889=EDGE_CURVE('',#3029,#3028,#2514,.T.);
#3890=EDGE_CURVE('',#3029,#3030,#277,.T.);
#3891=EDGE_CURVE('',#3030,#3031,#278,.T.);
#3892=EDGE_CURVE('',#3032,#3031,#2515,.T.);
#3893=EDGE_CURVE('',#3032,#3033,#279,.T.);
#3894=EDGE_CURVE('',#3033,#3034,#280,.T.);
#3895=EDGE_CURVE('',#3035,#3034,#2516,.T.);
#3896=EDGE_CURVE('',#3035,#3036,#281,.T.);
#3897=EDGE_CURVE('',#3036,#3037,#282,.T.);
#3898=EDGE_CURVE('',#3038,#3037,#2517,.T.);
#3899=EDGE_CURVE('',#3038,#3039,#283,.T.);
#3900=EDGE_CURVE('',#3039,#3040,#284,.T.);
#3901=EDGE_CURVE('',#3041,#3040,#2518,.T.);
#3902=EDGE_CURVE('',#3041,#3042,#285,.T.);
#3903=EDGE_CURVE('',#3042,#3043,#286,.T.);
#3904=EDGE_CURVE('',#3044,#3043,#2519,.T.);
#3905=EDGE_CURVE('',#3044,#3045,#287,.T.);
#3906=EDGE_CURVE('',#3045,#3046,#288,.T.);
#3907=EDGE_CURVE('',#3047,#3046,#2520,.T.);
#3908=EDGE_CURVE('',#3047,#3048,#289,.T.);
#3909=EDGE_CURVE('',#3048,#3049,#290,.T.);
#3910=EDGE_CURVE('',#3050,#3049,#2521,.T.);
#3911=EDGE_CURVE('',#3050,#3051,#291,.T.);
#3912=EDGE_CURVE('',#3051,#3052,#292,.T.);
#3913=EDGE_CURVE('',#3053,#3052,#2522,.T.);
#3914=EDGE_CURVE('',#3053,#3054,#293,.T.);
#3915=EDGE_CURVE('',#3054,#2996,#294,.T.);
#3916=EDGE_CURVE('',#2993,#3055,#1966,.T.);
#3917=EDGE_CURVE('',#3055,#3055,#2523,.T.);
#3918=EDGE_CURVE('',#3056,#3056,#2524,.T.);
#3919=EDGE_CURVE('',#3056,#3057,#1967,.T.);
#3920=EDGE_CURVE('',#3057,#3058,#2525,.T.);
#3921=EDGE_CURVE('',#3058,#3057,#2526,.T.);
#3922=EDGE_CURVE('',#3058,#2980,#1968,.T.);
#3923=EDGE_CURVE('',#2978,#3059,#1969,.T.);
#3924=EDGE_CURVE('',#3059,#3059,#2527,.T.);
#3925=EDGE_CURVE('',#3060,#3061,#437,.T.);
#3926=EDGE_CURVE('',#3062,#3060,#438,.T.);
#3927=EDGE_CURVE('',#3061,#3062,#2528,.T.);
#3928=EDGE_CURVE('',#3063,#3064,#439,.T.);
#3929=EDGE_CURVE('',#3065,#3063,#440,.T.);
#3930=EDGE_CURVE('',#3064,#3065,#2529,.T.);
#3931=EDGE_CURVE('',#3066,#3067,#441,.T.);
#3932=EDGE_CURVE('',#3068,#3066,#442,.T.);
#3933=EDGE_CURVE('',#3067,#3068,#2530,.T.);
#3934=EDGE_CURVE('',#3069,#3070,#443,.T.);
#3935=EDGE_CURVE('',#3071,#3069,#444,.T.);
#3936=EDGE_CURVE('',#3070,#3071,#2531,.T.);
#3937=EDGE_CURVE('',#3072,#3073,#445,.T.);
#3938=EDGE_CURVE('',#3074,#3072,#446,.T.);
#3939=EDGE_CURVE('',#3073,#3074,#2532,.T.);
#3940=EDGE_CURVE('',#3075,#3076,#447,.T.);
#3941=EDGE_CURVE('',#3077,#3075,#448,.T.);
#3942=EDGE_CURVE('',#3076,#3077,#2533,.T.);
#3943=EDGE_CURVE('',#3078,#3079,#449,.T.);
#3944=EDGE_CURVE('',#3080,#3078,#450,.T.);
#3945=EDGE_CURVE('',#3079,#3080,#2534,.T.);
#3946=EDGE_CURVE('',#3081,#3082,#451,.T.);
#3947=EDGE_CURVE('',#3083,#3081,#452,.T.);
#3948=EDGE_CURVE('',#3082,#3083,#2535,.T.);
#3949=EDGE_CURVE('',#3084,#3085,#453,.T.);
#3950=EDGE_CURVE('',#3086,#3084,#454,.T.);
#3951=EDGE_CURVE('',#3085,#3086,#2536,.T.);
#3952=EDGE_CURVE('',#3087,#3088,#455,.T.);
#3953=EDGE_CURVE('',#3089,#3087,#456,.T.);
#3954=EDGE_CURVE('',#3088,#3089,#2537,.T.);
#3955=EDGE_CURVE('',#3090,#3091,#457,.T.);
#3956=EDGE_CURVE('',#3092,#3090,#458,.T.);
#3957=EDGE_CURVE('',#3091,#3092,#2538,.T.);
#3958=EDGE_CURVE('',#3093,#3094,#459,.T.);
#3959=EDGE_CURVE('',#3095,#3093,#460,.T.);
#3960=EDGE_CURVE('',#3094,#3095,#2539,.T.);
#3961=EDGE_CURVE('',#3096,#3097,#461,.T.);
#3962=EDGE_CURVE('',#3098,#3096,#462,.T.);
#3963=EDGE_CURVE('',#3097,#3098,#2540,.T.);
#3964=EDGE_CURVE('',#3099,#3100,#463,.T.);
#3965=EDGE_CURVE('',#3101,#3099,#464,.T.);
#3966=EDGE_CURVE('',#3100,#3101,#2541,.T.);
#3967=EDGE_CURVE('',#3102,#3103,#465,.T.);
#3968=EDGE_CURVE('',#3104,#3102,#466,.T.);
#3969=EDGE_CURVE('',#3103,#3104,#2542,.T.);
#3970=EDGE_CURVE('',#3105,#3106,#467,.T.);
#3971=EDGE_CURVE('',#3107,#3105,#468,.T.);
#3972=EDGE_CURVE('',#3106,#3107,#2543,.T.);
#3973=EDGE_CURVE('',#3108,#3109,#469,.T.);
#3974=EDGE_CURVE('',#3110,#3108,#470,.T.);
#3975=EDGE_CURVE('',#3109,#3110,#2544,.T.);
#3976=EDGE_CURVE('',#3111,#3112,#471,.T.);
#3977=EDGE_CURVE('',#3113,#3111,#472,.T.);
#3978=EDGE_CURVE('',#3112,#3113,#2545,.T.);
#3979=EDGE_CURVE('',#3114,#3115,#473,.T.);
#3980=EDGE_CURVE('',#3116,#3114,#474,.T.);
#3981=EDGE_CURVE('',#3115,#3116,#2546,.T.);
#3982=EDGE_CURVE('',#3117,#3117,#2547,.T.);
#3983=EDGE_CURVE('',#3117,#3118,#1970,.T.);
#3984=EDGE_CURVE('',#3118,#3118,#2548,.T.);
#3985=EDGE_CURVE('',#3118,#3119,#1971,.T.);
#3986=EDGE_CURVE('',#3119,#3119,#2549,.T.);
#3987=EDGE_CURVE('',#3120,#3121,#475,.T.);
#3988=EDGE_CURVE('',#3122,#3120,#476,.T.);
#3989=EDGE_CURVE('',#3121,#3122,#2550,.T.);
#3990=EDGE_CURVE('',#3054,#3120,#1972,.T.);
#3991=EDGE_CURVE('',#3123,#3053,#477,.T.);
#3992=EDGE_CURVE('',#3123,#3122,#295,.T.);
#3993=EDGE_CURVE('',#2997,#3114,#1973,.T.);
#3994=EDGE_CURVE('',#3124,#2995,#478,.T.);
#3995=EDGE_CURVE('',#3124,#3116,#296,.T.);
#3996=EDGE_CURVE('',#3000,#3111,#1974,.T.);
#3997=EDGE_CURVE('',#3125,#2999,#479,.T.);
#3998=EDGE_CURVE('',#3125,#3113,#297,.T.);
#3999=EDGE_CURVE('',#3003,#3108,#1975,.T.);
#4000=EDGE_CURVE('',#3126,#3002,#480,.T.);
#4001=EDGE_CURVE('',#3126,#3110,#298,.T.);
#4002=EDGE_CURVE('',#3006,#3105,#1976,.T.);
#4003=EDGE_CURVE('',#3127,#3005,#481,.T.);
#4004=EDGE_CURVE('',#3127,#3107,#299,.T.);
#4005=EDGE_CURVE('',#3009,#3102,#1977,.T.);
#4006=EDGE_CURVE('',#3128,#3008,#482,.T.);
#4007=EDGE_CURVE('',#3128,#3104,#300,.T.);
#4008=EDGE_CURVE('',#3012,#3099,#1978,.T.);
#4009=EDGE_CURVE('',#3129,#3011,#483,.T.);
#4010=EDGE_CURVE('',#3129,#3101,#301,.T.);
#4011=EDGE_CURVE('',#3015,#3096,#1979,.T.);
#4012=EDGE_CURVE('',#3130,#3014,#484,.T.);
#4013=EDGE_CURVE('',#3130,#3098,#302,.T.);
#4014=EDGE_CURVE('',#3018,#3093,#1980,.T.);
#4015=EDGE_CURVE('',#3131,#3017,#485,.T.);
#4016=EDGE_CURVE('',#3131,#3095,#303,.T.);
#4017=EDGE_CURVE('',#3021,#3090,#1981,.T.);
#4018=EDGE_CURVE('',#3132,#3020,#486,.T.);
#4019=EDGE_CURVE('',#3132,#3092,#304,.T.);
#4020=EDGE_CURVE('',#3024,#3087,#1982,.T.);
#4021=EDGE_CURVE('',#3133,#3023,#487,.T.);
#4022=EDGE_CURVE('',#3133,#3089,#305,.T.);
#4023=EDGE_CURVE('',#3027,#3084,#1983,.T.);
#4024=EDGE_CURVE('',#3134,#3026,#488,.T.);
#4025=EDGE_CURVE('',#3134,#3086,#306,.T.);
#4026=EDGE_CURVE('',#3030,#3081,#1984,.T.);
#4027=EDGE_CURVE('',#3135,#3029,#489,.T.);
#4028=EDGE_CURVE('',#3135,#3083,#307,.T.);
#4029=EDGE_CURVE('',#3033,#3078,#1985,.T.);
#4030=EDGE_CURVE('',#3136,#3032,#490,.T.);
#4031=EDGE_CURVE('',#3136,#3080,#308,.T.);
#4032=EDGE_CURVE('',#3036,#3075,#1986,.T.);
#4033=EDGE_CURVE('',#3137,#3035,#491,.T.);
#4034=EDGE_CURVE('',#3137,#3077,#309,.T.);
#4035=EDGE_CURVE('',#3039,#3072,#1987,.T.);
#4036=EDGE_CURVE('',#3138,#3038,#492,.T.);
#4037=EDGE_CURVE('',#3138,#3074,#310,.T.);
#4038=EDGE_CURVE('',#3042,#3069,#1988,.T.);
#4039=EDGE_CURVE('',#3139,#3041,#493,.T.);
#4040=EDGE_CURVE('',#3139,#3071,#311,.T.);
#4041=EDGE_CURVE('',#3045,#3066,#1989,.T.);
#4042=EDGE_CURVE('',#3140,#3044,#494,.T.);
#4043=EDGE_CURVE('',#3140,#3068,#312,.T.);
#4044=EDGE_CURVE('',#3048,#3063,#1990,.T.);
#4045=EDGE_CURVE('',#3141,#3047,#495,.T.);
#4046=EDGE_CURVE('',#3141,#3065,#313,.T.);
#4047=EDGE_CURVE('',#3051,#3060,#1991,.T.);
#4048=EDGE_CURVE('',#3142,#3050,#496,.T.);
#4049=EDGE_CURVE('',#3142,#3062,#314,.T.);
#4050=EDGE_CURVE('',#3121,#3143,#315,.T.);
#4051=EDGE_CURVE('',#2996,#3143,#497,.T.);
#4052=EDGE_CURVE('',#3143,#3123,#2551,.T.);
#4053=EDGE_CURVE('',#3117,#3144,#1992,.T.);
#4054=EDGE_CURVE('',#3144,#3132,#2552,.T.);
#4055=EDGE_CURVE('',#3019,#3145,#498,.T.);
#4056=EDGE_CURVE('',#3145,#3131,#2553,.T.);
#4057=EDGE_CURVE('',#3016,#3146,#499,.T.);
#4058=EDGE_CURVE('',#3146,#3130,#2554,.T.);
#4059=EDGE_CURVE('',#3013,#3147,#500,.T.);
#4060=EDGE_CURVE('',#3147,#3129,#2555,.T.);
#4061=EDGE_CURVE('',#3010,#3148,#501,.T.);
#4062=EDGE_CURVE('',#3148,#3128,#2556,.T.);
#4063=EDGE_CURVE('',#3007,#3149,#502,.T.);
#4064=EDGE_CURVE('',#3149,#3127,#2557,.T.);
#4065=EDGE_CURVE('',#3004,#3150,#503,.T.);
#4066=EDGE_CURVE('',#3150,#3126,#2558,.T.);
#4067=EDGE_CURVE('',#3001,#3151,#504,.T.);
#4068=EDGE_CURVE('',#3151,#3125,#2559,.T.);
#4069=EDGE_CURVE('',#2998,#3152,#505,.T.);
#4070=EDGE_CURVE('',#3152,#3124,#2560,.T.);
#4071=EDGE_CURVE('',#3052,#3153,#506,.T.);
#4072=EDGE_CURVE('',#3153,#3142,#2561,.T.);
#4073=EDGE_CURVE('',#3049,#3154,#507,.T.);
#4074=EDGE_CURVE('',#3154,#3141,#2562,.T.);
#4075=EDGE_CURVE('',#3046,#3155,#508,.T.);
#4076=EDGE_CURVE('',#3155,#3140,#2563,.T.);
#4077=EDGE_CURVE('',#3043,#3156,#509,.T.);
#4078=EDGE_CURVE('',#3156,#3139,#2564,.T.);
#4079=EDGE_CURVE('',#3040,#3157,#510,.T.);
#4080=EDGE_CURVE('',#3157,#3138,#2565,.T.);
#4081=EDGE_CURVE('',#3037,#3158,#511,.T.);
#4082=EDGE_CURVE('',#3158,#3137,#2566,.T.);
#4083=EDGE_CURVE('',#3034,#3159,#512,.T.);
#4084=EDGE_CURVE('',#3159,#3136,#2567,.T.);
#4085=EDGE_CURVE('',#3031,#3160,#513,.T.);
#4086=EDGE_CURVE('',#3160,#3135,#2568,.T.);
#4087=EDGE_CURVE('',#3028,#3161,#514,.T.);
#4088=EDGE_CURVE('',#3161,#3134,#2569,.T.);
#4089=EDGE_CURVE('',#3025,#3162,#515,.T.);
#4090=EDGE_CURVE('',#3162,#3133,#2570,.T.);
#4091=EDGE_CURVE('',#3022,#3163,#516,.T.);
#4092=EDGE_CURVE('',#3163,#3144,#2571,.T.);
#4093=EDGE_CURVE('',#3115,#3152,#316,.T.);
#4094=EDGE_CURVE('',#3112,#3151,#317,.T.);
#4095=EDGE_CURVE('',#3109,#3150,#318,.T.);
#4096=EDGE_CURVE('',#3106,#3149,#319,.T.);
#4097=EDGE_CURVE('',#3103,#3148,#320,.T.);
#4098=EDGE_CURVE('',#3100,#3147,#321,.T.);
#4099=EDGE_CURVE('',#3097,#3146,#322,.T.);
#4100=EDGE_CURVE('',#3094,#3145,#323,.T.);
#4101=EDGE_CURVE('',#3091,#3163,#324,.T.);
#4102=EDGE_CURVE('',#3088,#3162,#325,.T.);
#4103=EDGE_CURVE('',#3085,#3161,#326,.T.);
#4104=EDGE_CURVE('',#3082,#3160,#327,.T.);
#4105=EDGE_CURVE('',#3079,#3159,#328,.T.);
#4106=EDGE_CURVE('',#3076,#3158,#329,.T.);
#4107=EDGE_CURVE('',#3073,#3157,#330,.T.);
#4108=EDGE_CURVE('',#3070,#3156,#331,.T.);
#4109=EDGE_CURVE('',#3067,#3155,#332,.T.);
#4110=EDGE_CURVE('',#3064,#3154,#333,.T.);
#4111=EDGE_CURVE('',#3061,#3153,#334,.T.);
#4112=EDGE_CURVE('',#3164,#3165,#2572,.T.);
#4113=EDGE_CURVE('',#3164,#3166,#1993,.T.);
#4114=EDGE_CURVE('',#3165,#3166,#2573,.T.);
#4115=EDGE_CURVE('',#3167,#3168,#2574,.T.);
#4116=EDGE_CURVE('',#3167,#3169,#1994,.T.);
#4117=EDGE_CURVE('',#3168,#3169,#2575,.T.);
#4118=EDGE_CURVE('',#3169,#3164,#1995,.T.);
#4119=EDGE_CURVE('',#3166,#3167,#1996,.T.);
#4120=EDGE_CURVE('',#3170,#3171,#2576,.T.);
#4121=EDGE_CURVE('',#3170,#3171,#1997,.T.);
#4122=EDGE_CURVE('',#3172,#3170,#1998,.T.);
#4123=EDGE_CURVE('',#3173,#3172,#1999,.T.);
#4124=EDGE_CURVE('',#3171,#3173,#2000,.T.);
#4125=EDGE_CURVE('',#3173,#3172,#2577,.T.);
#4126=EDGE_CURVE('',#3174,#3175,#2001,.T.);
#4127=EDGE_CURVE('',#3175,#3175,#2578,.T.);
#4128=EDGE_CURVE('',#3175,#3176,#2002,.T.);
#4129=EDGE_CURVE('',#3176,#3176,#2579,.T.);
#4130=EDGE_CURVE('',#3177,#3177,#2580,.T.);
#4131=EDGE_CURVE('',#3177,#3178,#2003,.T.);
#4132=EDGE_CURVE('',#3178,#3178,#2581,.T.);
#4133=EDGE_CURVE('',#3178,#3179,#2004,.T.);
#4134=EDGE_CURVE('',#3180,#3180,#2582,.T.);
#4135=EDGE_CURVE('',#3181,#3181,#2583,.T.);
#4136=EDGE_CURVE('',#3181,#3180,#2005,.T.);
#4137=EDGE_CURVE('',#3182,#3182,#2584,.T.);
#4138=EDGE_CURVE('',#3182,#3168,#2006,.T.);
#4139=EDGE_CURVE('',#3165,#3181,#2007,.T.);
#4140=EDGE_CURVE('',#3183,#3183,#2585,.T.);
#4141=EDGE_CURVE('',#3183,#3182,#2008,.T.);
#4142=EDGE_CURVE('',#3184,#3185,#2586,.T.);
#4143=EDGE_CURVE('',#3184,#3186,#2009,.T.);
#4144=EDGE_CURVE('',#3185,#3186,#2587,.T.);
#4145=EDGE_CURVE('',#3187,#3188,#2588,.T.);
#4146=EDGE_CURVE('',#3187,#3189,#2010,.T.);
#4147=EDGE_CURVE('',#3188,#3189,#2589,.T.);
#4148=EDGE_CURVE('',#3189,#3184,#2011,.T.);
#4149=EDGE_CURVE('',#3186,#3187,#2012,.T.);
#4150=EDGE_CURVE('',#3190,#3191,#2590,.T.);
#4151=EDGE_CURVE('',#3190,#3191,#2013,.T.);
#4152=EDGE_CURVE('',#3192,#3190,#2014,.T.);
#4153=EDGE_CURVE('',#3193,#3192,#2015,.T.);
#4154=EDGE_CURVE('',#3191,#3193,#2016,.T.);
#4155=EDGE_CURVE('',#3193,#3192,#2591,.T.);
#4156=EDGE_CURVE('',#3194,#3195,#2017,.T.);
#4157=EDGE_CURVE('',#3195,#3195,#2592,.T.);
#4158=EDGE_CURVE('',#3195,#3196,#2018,.T.);
#4159=EDGE_CURVE('',#3196,#3196,#2593,.T.);
#4160=EDGE_CURVE('',#3197,#3197,#2594,.T.);
#4161=EDGE_CURVE('',#3197,#3198,#2019,.T.);
#4162=EDGE_CURVE('',#3198,#3198,#2595,.T.);
#4163=EDGE_CURVE('',#3198,#3199,#2020,.T.);
#4164=EDGE_CURVE('',#3200,#3200,#2596,.T.);
#4165=EDGE_CURVE('',#3201,#3201,#2597,.T.);
#4166=EDGE_CURVE('',#3201,#3200,#2021,.T.);
#4167=EDGE_CURVE('',#3202,#3202,#2598,.T.);
#4168=EDGE_CURVE('',#3202,#3188,#2022,.T.);
#4169=EDGE_CURVE('',#3185,#3201,#2023,.T.);
#4170=EDGE_CURVE('',#3203,#3203,#2599,.T.);
#4171=EDGE_CURVE('',#3203,#3202,#2024,.T.);
#4172=EDGE_CURVE('',#3204,#3205,#2600,.T.);
#4173=EDGE_CURVE('',#3206,#3207,#517,.T.);
#4174=EDGE_CURVE('',#3208,#3206,#518,.T.);
#4175=EDGE_CURVE('',#3209,#3208,#519,.T.);
#4176=EDGE_CURVE('',#3207,#3209,#520,.T.);
#4177=EDGE_CURVE('',#3210,#3211,#521,.T.);
#4178=EDGE_CURVE('',#3212,#3210,#522,.T.);
#4179=EDGE_CURVE('',#3213,#3212,#523,.T.);
#4180=EDGE_CURVE('',#3211,#3213,#524,.T.);
#4181=EDGE_CURVE('',#3214,#3214,#2601,.T.);
#4182=EDGE_CURVE('',#3214,#3215,#2025,.T.);
#4183=EDGE_CURVE('',#3215,#3216,#525,.T.);
#4184=EDGE_CURVE('',#3217,#3216,#2602,.T.);
#4185=EDGE_CURVE('',#3217,#3218,#526,.T.);
#4186=EDGE_CURVE('',#3219,#3218,#2603,.T.);
#4187=EDGE_CURVE('',#3219,#3220,#527,.T.);
#4188=EDGE_CURVE('',#3221,#3220,#2604,.T.);
#4189=EDGE_CURVE('',#3221,#3222,#528,.T.);
#4190=EDGE_CURVE('',#3223,#3222,#2605,.T.);
#4191=EDGE_CURVE('',#3223,#3224,#529,.T.);
#4192=EDGE_CURVE('',#3225,#3224,#2606,.T.);
#4193=EDGE_CURVE('',#3225,#3226,#530,.T.);
#4194=EDGE_CURVE('',#3209,#3226,#2607,.T.);
#4195=EDGE_CURVE('',#3227,#3208,#2608,.T.);
#4196=EDGE_CURVE('',#3227,#3228,#531,.T.);
#4197=EDGE_CURVE('',#3229,#3228,#2609,.T.);
#4198=EDGE_CURVE('',#3229,#3230,#532,.T.);
#4199=EDGE_CURVE('',#3231,#3230,#2610,.T.);
#4200=EDGE_CURVE('',#3231,#3232,#533,.T.);
#4201=EDGE_CURVE('',#3233,#3232,#2611,.T.);
#4202=EDGE_CURVE('',#3233,#3215,#534,.T.);
#4203=EDGE_CURVE('',#3234,#3206,#2612,.T.);
#4204=EDGE_CURVE('',#3234,#3227,#535,.T.);
#4205=EDGE_CURVE('',#3235,#3212,#2613,.T.);
#4206=EDGE_CURVE('',#3235,#3236,#536,.T.);
#4207=EDGE_CURVE('',#3237,#3236,#2614,.T.);
#4208=EDGE_CURVE('',#3237,#3238,#537,.T.);
#4209=EDGE_CURVE('',#3239,#3238,#2615,.T.);
#4210=EDGE_CURVE('',#3239,#3240,#538,.T.);
#4211=EDGE_CURVE('',#3241,#3240,#2616,.T.);
#4212=EDGE_CURVE('',#3241,#3242,#539,.T.);
#4213=EDGE_CURVE('',#3242,#3243,#2026,.T.);
#4214=EDGE_CURVE('',#3243,#3243,#2617,.T.);
#4215=EDGE_CURVE('',#3242,#3244,#540,.T.);
#4216=EDGE_CURVE('',#3245,#3244,#2618,.T.);
#4217=EDGE_CURVE('',#3245,#3246,#541,.T.);
#4218=EDGE_CURVE('',#3247,#3246,#2619,.T.);
#4219=EDGE_CURVE('',#3247,#3248,#542,.T.);
#4220=EDGE_CURVE('',#3249,#3248,#2620,.T.);
#4221=EDGE_CURVE('',#3249,#3250,#543,.T.);
#4222=EDGE_CURVE('',#3251,#3250,#2621,.T.);
#4223=EDGE_CURVE('',#3251,#3252,#544,.T.);
#4224=EDGE_CURVE('',#3253,#3252,#2622,.T.);
#4225=EDGE_CURVE('',#3253,#3254,#545,.T.);
#4226=EDGE_CURVE('',#3213,#3254,#2623,.T.);
#4227=EDGE_CURVE('',#3255,#3210,#2624,.T.);
#4228=EDGE_CURVE('',#3255,#3235,#546,.T.);
#4229=EDGE_CURVE('',#3256,#3257,#2625,.T.);
#4230=EDGE_CURVE('',#3258,#3234,#547,.T.);
#4231=EDGE_CURVE('',#3228,#3258,#548,.T.);
#4232=EDGE_CURVE('',#3259,#3255,#549,.T.);
#4233=EDGE_CURVE('',#3236,#3259,#550,.T.);
#4234=EDGE_CURVE('',#3260,#3258,#2626,.T.);
#4235=EDGE_CURVE('',#3260,#3229,#551,.T.);
#4236=EDGE_CURVE('',#3261,#3259,#2627,.T.);
#4237=EDGE_CURVE('',#3261,#3237,#552,.T.);
#4238=EDGE_CURVE('',#3262,#3263,#2628,.T.);
#4239=EDGE_CURVE('',#3264,#3260,#553,.T.);
#4240=EDGE_CURVE('',#3230,#3264,#554,.T.);
#4241=EDGE_CURVE('',#3265,#3261,#555,.T.);
#4242=EDGE_CURVE('',#3238,#3265,#556,.T.);
#4243=EDGE_CURVE('',#3266,#3264,#2629,.T.);
#4244=EDGE_CURVE('',#3266,#3231,#557,.T.);
#4245=EDGE_CURVE('',#3267,#3265,#2630,.T.);
#4246=EDGE_CURVE('',#3267,#3239,#558,.T.);
#4247=EDGE_CURVE('',#3268,#3269,#2631,.T.);
#4248=EDGE_CURVE('',#3270,#3266,#559,.T.);
#4249=EDGE_CURVE('',#3232,#3270,#560,.T.);
#4250=EDGE_CURVE('',#3271,#3267,#561,.T.);
#4251=EDGE_CURVE('',#3240,#3271,#562,.T.);
#4252=EDGE_CURVE('',#3272,#3270,#2632,.T.);
#4253=EDGE_CURVE('',#3272,#3233,#563,.T.);
#4254=EDGE_CURVE('',#3273,#3271,#2633,.T.);
#4255=EDGE_CURVE('',#3273,#3241,#564,.T.);
#4256=EDGE_CURVE('',#3274,#3275,#2634,.T.);
#4257=EDGE_CURVE('',#3276,#3277,#565,.T.);
#4258=EDGE_CURVE('',#3216,#3276,#566,.T.);
#4259=EDGE_CURVE('',#3277,#3272,#567,.T.);
#4260=EDGE_CURVE('',#3278,#3279,#568,.T.);
#4261=EDGE_CURVE('',#3244,#3278,#569,.T.);
#4262=EDGE_CURVE('',#3279,#3273,#570,.T.);
#4263=EDGE_CURVE('',#3280,#3276,#2635,.T.);
#4264=EDGE_CURVE('',#3280,#3217,#571,.T.);
#4265=EDGE_CURVE('',#3281,#3278,#2636,.T.);
#4266=EDGE_CURVE('',#3281,#3245,#572,.T.);
#4267=EDGE_CURVE('',#3282,#3283,#2637,.T.);
#4268=EDGE_CURVE('',#3284,#3280,#573,.T.);
#4269=EDGE_CURVE('',#3218,#3284,#574,.T.);
#4270=EDGE_CURVE('',#3285,#3281,#575,.T.);
#4271=EDGE_CURVE('',#3246,#3285,#576,.T.);
#4272=EDGE_CURVE('',#3286,#3284,#2638,.T.);
#4273=EDGE_CURVE('',#3286,#3219,#577,.T.);
#4274=EDGE_CURVE('',#3287,#3285,#2639,.T.);
#4275=EDGE_CURVE('',#3287,#3247,#578,.T.);
#4276=EDGE_CURVE('',#3288,#3289,#2640,.T.);
#4277=EDGE_CURVE('',#3290,#3286,#579,.T.);
#4278=EDGE_CURVE('',#3220,#3290,#580,.T.);
#4279=EDGE_CURVE('',#3291,#3287,#581,.T.);
#4280=EDGE_CURVE('',#3248,#3291,#582,.T.);
#4281=EDGE_CURVE('',#3292,#3290,#2641,.T.);
#4282=EDGE_CURVE('',#3292,#3221,#583,.T.);
#4283=EDGE_CURVE('',#3293,#3291,#2642,.T.);
#4284=EDGE_CURVE('',#3293,#3249,#584,.T.);
#4285=EDGE_CURVE('',#3294,#3295,#2643,.T.);
#4286=EDGE_CURVE('',#3296,#3292,#585,.T.);
#4287=EDGE_CURVE('',#3222,#3296,#586,.T.);
#4288=EDGE_CURVE('',#3297,#3293,#587,.T.);
#4289=EDGE_CURVE('',#3250,#3297,#588,.T.);
#4290=EDGE_CURVE('',#3298,#3296,#2644,.T.);
#4291=EDGE_CURVE('',#3298,#3223,#589,.T.);
#4292=EDGE_CURVE('',#3299,#3297,#2645,.T.);
#4293=EDGE_CURVE('',#3299,#3251,#590,.T.);
#4294=EDGE_CURVE('',#3300,#3301,#2646,.T.);
#4295=EDGE_CURVE('',#3302,#3298,#591,.T.);
#4296=EDGE_CURVE('',#3224,#3302,#592,.T.);
#4297=EDGE_CURVE('',#3303,#3299,#593,.T.);
#4298=EDGE_CURVE('',#3252,#3303,#594,.T.);
#4299=EDGE_CURVE('',#3207,#3304,#2647,.T.);
#4300=EDGE_CURVE('',#3304,#3305,#595,.T.);
#4301=EDGE_CURVE('',#3305,#3302,#2648,.T.);
#4302=EDGE_CURVE('',#3277,#3306,#2027,.T.);
#4303=EDGE_CURVE('',#3306,#3306,#2649,.T.);
#4304=EDGE_CURVE('',#3226,#3304,#596,.T.);
#4305=EDGE_CURVE('',#3307,#3307,#2650,.T.);
#4306=EDGE_CURVE('',#3307,#3279,#2028,.T.);
#4307=EDGE_CURVE('',#3211,#3308,#2651,.T.);
#4308=EDGE_CURVE('',#3308,#3309,#597,.T.);
#4309=EDGE_CURVE('',#3309,#3303,#2652,.T.);
#4310=EDGE_CURVE('',#3254,#3308,#598,.T.);
#4311=EDGE_CURVE('',#3310,#3311,#2653,.T.);
#4312=EDGE_CURVE('',#3309,#3253,#599,.T.);
#4313=EDGE_CURVE('',#3305,#3225,#600,.T.);
#4314=EDGE_CURVE('',#3312,#3312,#2654,.T.);
#4315=EDGE_CURVE('',#3313,#3313,#2655,.T.);
#4316=EDGE_CURVE('',#3313,#3312,#2029,.T.);
#4317=EDGE_CURVE('',#3314,#3314,#2656,.T.);
#4318=EDGE_CURVE('',#3314,#3313,#2030,.T.);
#4319=EDGE_CURVE('',#3315,#3315,#2657,.T.);
#4320=EDGE_CURVE('',#3315,#3314,#2031,.T.);
#4321=EDGE_CURVE('',#3316,#3316,#2658,.T.);
#4322=EDGE_CURVE('',#3316,#3214,#2032,.T.);
#4323=EDGE_CURVE('',#3317,#3317,#2659,.T.);
#4324=EDGE_CURVE('',#3317,#3318,#2033,.T.);
#4325=EDGE_CURVE('',#3318,#3318,#2660,.T.);
#4326=EDGE_CURVE('',#3318,#3319,#2034,.T.);
#4327=EDGE_CURVE('',#3319,#3319,#2661,.T.);
#4328=EDGE_CURVE('',#3319,#3320,#2035,.T.);
#4329=EDGE_CURVE('',#3320,#3320,#2662,.T.);
#4330=EDGE_CURVE('',#3321,#3321,#2663,.T.);
#4331=EDGE_CURVE('',#3322,#3322,#2664,.T.);
#4332=EDGE_CURVE('',#3323,#3323,#2665,.T.);
#4333=EDGE_CURVE('',#3323,#3321,#2036,.T.);
#4334=EDGE_CURVE('',#3324,#3324,#2666,.T.);
#4335=EDGE_CURVE('',#3324,#3325,#2037,.T.);
#4336=EDGE_CURVE('',#3325,#3325,#2667,.T.);
#4337=EDGE_CURVE('',#3326,#3326,#2668,.T.);
#4338=EDGE_CURVE('',#3327,#3327,#2669,.T.);
#4339=EDGE_CURVE('',#3327,#3326,#2038,.T.);
#4340=EDGE_CURVE('',#3328,#3328,#2670,.T.);
#4341=EDGE_CURVE('',#3328,#3327,#2039,.T.);
#4342=EDGE_CURVE('',#3329,#3329,#2671,.T.);
#4343=EDGE_CURVE('',#3329,#3328,#2040,.T.);
#4344=EDGE_CURVE('',#3330,#3330,#2672,.T.);
#4345=EDGE_CURVE('',#3330,#3331,#2041,.T.);
#4346=EDGE_CURVE('',#3331,#3331,#2673,.T.);
#4347=EDGE_CURVE('',#3332,#3332,#2674,.T.);
#4348=EDGE_CURVE('',#3333,#3333,#2675,.T.);
#4349=EDGE_CURVE('',#3333,#3332,#2042,.T.);
#4350=EDGE_CURVE('',#3334,#3334,#2676,.T.);
#4351=EDGE_CURVE('',#3334,#3335,#2043,.T.);
#4352=EDGE_CURVE('',#3335,#3335,#2677,.T.);
#4353=EDGE_CURVE('',#3335,#3336,#2044,.T.);
#4354=EDGE_CURVE('',#3336,#3336,#2678,.T.);
#4355=EDGE_CURVE('',#3336,#3322,#2045,.T.);
#4356=EDGE_CURVE('',#3337,#3337,#2679,.T.);
#4357=EDGE_CURVE('',#3337,#3338,#2046,.T.);
#4358=EDGE_CURVE('',#3338,#3338,#2680,.T.);
#4359=EDGE_CURVE('',#3339,#3339,#2681,.T.);
#4360=EDGE_CURVE('',#3339,#3340,#2047,.T.);
#4361=EDGE_CURVE('',#3340,#3340,#2682,.T.);
#4362=EDGE_CURVE('',#3341,#3342,#2048,.T.);
#4363=EDGE_CURVE('',#3341,#3343,#601,.T.);
#4364=EDGE_CURVE('',#3343,#3344,#2683,.T.);
#4365=EDGE_CURVE('',#3344,#3342,#602,.T.);
#4366=EDGE_CURVE('',#3345,#3346,#2049,.T.);
#4367=EDGE_CURVE('',#3345,#3341,#603,.T.);
#4368=EDGE_CURVE('',#3342,#3346,#604,.T.);
#4369=EDGE_CURVE('',#3347,#3348,#2050,.T.);
#4370=EDGE_CURVE('',#3347,#3345,#605,.T.);
#4371=EDGE_CURVE('',#3346,#3348,#606,.T.);
#4372=EDGE_CURVE('',#3349,#3350,#2051,.T.);
#4373=EDGE_CURVE('',#3349,#3347,#607,.T.);
#4374=EDGE_CURVE('',#3348,#3350,#608,.T.);
#4375=EDGE_CURVE('',#3351,#3352,#2052,.T.);
#4376=EDGE_CURVE('',#3351,#3349,#609,.T.);
#4377=EDGE_CURVE('',#3350,#3352,#610,.T.);
#4378=EDGE_CURVE('',#3353,#3354,#2053,.T.);
#4379=EDGE_CURVE('',#3353,#3355,#611,.T.);
#4380=EDGE_CURVE('',#3356,#3355,#2684,.T.);
#4381=EDGE_CURVE('',#3354,#3356,#612,.T.);
#4382=EDGE_CURVE('',#3357,#3358,#2054,.T.);
#4383=EDGE_CURVE('',#3357,#3353,#613,.T.);
#4384=EDGE_CURVE('',#3358,#3354,#614,.T.);
#4385=EDGE_CURVE('',#3359,#3360,#2055,.T.);
#4386=EDGE_CURVE('',#3359,#3357,#615,.T.);
#4387=EDGE_CURVE('',#3360,#3358,#616,.T.);
#4388=EDGE_CURVE('',#3361,#3362,#2056,.T.);
#4389=EDGE_CURVE('',#3361,#3359,#617,.T.);
#4390=EDGE_CURVE('',#3362,#3360,#618,.T.);
#4391=EDGE_CURVE('',#3355,#3363,#619,.T.);
#4392=EDGE_CURVE('',#3364,#3363,#2685,.F.);
#4393=EDGE_CURVE('',#3365,#3364,#2686,.F.);
#4394=EDGE_CURVE('',#3365,#3356,#620,.T.);
#4395=EDGE_CURVE('',#3352,#3365,#621,.T.);
#4396=EDGE_CURVE('',#3366,#3344,#622,.T.);
#4397=EDGE_CURVE('',#3366,#3362,#623,.T.);
#4398=EDGE_CURVE('',#3344,#3367,#2687,.T.);
#4399=EDGE_CURVE('',#3367,#3343,#2688,.T.);
#4400=EDGE_CURVE('',#3343,#3368,#624,.T.);
#4401=EDGE_CURVE('',#3368,#3366,#2689,.T.);
#4402=EDGE_CURVE('',#3368,#3361,#625,.T.);
#4403=EDGE_CURVE('',#3363,#3351,#626,.T.);
#4404=EDGE_CURVE('',#3369,#3370,#2057,.T.);
#4405=EDGE_CURVE('',#3370,#3370,#2690,.T.);
#4406=EDGE_CURVE('',#3371,#3372,#2058,.T.);
#4407=EDGE_CURVE('',#3373,#3371,#2059,.T.);
#4408=EDGE_CURVE('',#3374,#3373,#2060,.T.);
#4409=EDGE_CURVE('',#3374,#3372,#2061,.T.);
#4410=EDGE_CURVE('',#3372,#3375,#2062,.T.);
#4411=EDGE_CURVE('',#3376,#3374,#2063,.T.);
#4412=EDGE_CURVE('',#3376,#3375,#2064,.T.);
#4413=EDGE_CURVE('',#3375,#3377,#2065,.T.);
#4414=EDGE_CURVE('',#3378,#3376,#2066,.T.);
#4415=EDGE_CURVE('',#3378,#3377,#2067,.T.);
#4416=EDGE_CURVE('',#3377,#3379,#2068,.T.);
#4417=EDGE_CURVE('',#3380,#3378,#2069,.T.);
#4418=EDGE_CURVE('',#3380,#3379,#2070,.T.);
#4419=EDGE_CURVE('',#3379,#3381,#2071,.T.);
#4420=EDGE_CURVE('',#3382,#3380,#2072,.T.);
#4421=EDGE_CURVE('',#3382,#3381,#2073,.T.);
#4422=EDGE_CURVE('',#3381,#3371,#2074,.T.);
#4423=EDGE_CURVE('',#3373,#3382,#2075,.T.);
#4424=EDGE_CURVE('',#3383,#3383,#2691,.T.);
#4425=EDGE_CURVE('',#3367,#3383,#2076,.T.);
#4426=EDGE_CURVE('',#3363,#3365,#2692,.F.);
#4427=EDGE_CURVE('',#3384,#3384,#2693,.T.);
#4428=EDGE_CURVE('',#3384,#3364,#2077,.T.);
#4429=EDGE_CURVE('',#3385,#3385,#2694,.T.);
#4430=EDGE_CURVE('',#3385,#3386,#2078,.T.);
#4431=EDGE_CURVE('',#3386,#3386,#2695,.T.);
#4432=EDGE_CURVE('',#3387,#3387,#2696,.T.);
#4433=EDGE_CURVE('',#3387,#3388,#2079,.T.);
#4434=EDGE_CURVE('',#3388,#3388,#2697,.T.);
#4435=EDGE_CURVE('',#3389,#3390,#2080,.T.);
#4436=EDGE_CURVE('',#3390,#3391,#2698,.T.);
#4437=EDGE_CURVE('',#3391,#3392,#2081,.T.);
#4438=EDGE_CURVE('',#3389,#3392,#2699,.T.);
#4439=EDGE_CURVE('',#3393,#3390,#2082,.T.);
#4440=EDGE_CURVE('',#3394,#3393,#2083,.T.);
#4441=EDGE_CURVE('',#3395,#3394,#2084,.T.);
#4442=EDGE_CURVE('',#3395,#3396,#2700,.T.);
#4443=EDGE_CURVE('',#3396,#3397,#2085,.T.);
#4444=EDGE_CURVE('',#3397,#3398,#2086,.T.);
#4445=EDGE_CURVE('',#3398,#3391,#2087,.T.);
#4446=EDGE_CURVE('',#3399,#3396,#2088,.T.);
#4447=EDGE_CURVE('',#3400,#3399,#2089,.T.);
#4448=EDGE_CURVE('',#3397,#3400,#2090,.T.);
#4449=EDGE_CURVE('',#3401,#3400,#2091,.T.);
#4450=EDGE_CURVE('',#3398,#3401,#2092,.T.);
#4451=EDGE_CURVE('',#3392,#3401,#2093,.T.);
#4452=EDGE_CURVE('',#3402,#3389,#2094,.T.);
#4453=EDGE_CURVE('',#3393,#3402,#2095,.T.);
#4454=EDGE_CURVE('',#3395,#3403,#2096,.T.);
#4455=EDGE_CURVE('',#3394,#3404,#2097,.T.);
#4456=EDGE_CURVE('',#3403,#3404,#2098,.T.);
#4457=EDGE_CURVE('',#3404,#3402,#2099,.T.);
#4458=EDGE_CURVE('',#3403,#3399,#2701,.T.);
#4459=ORIENTED_EDGE('',*,*,#3405,.F.);
#4460=ORIENTED_EDGE('',*,*,#3406,.T.);
#4461=ORIENTED_EDGE('',*,*,#3407,.T.);
#4462=ORIENTED_EDGE('',*,*,#3406,.F.);
#4463=ORIENTED_EDGE('',*,*,#3408,.T.);
#4464=ORIENTED_EDGE('',*,*,#3407,.F.);
#4465=ORIENTED_EDGE('',*,*,#3408,.F.);
#4466=ORIENTED_EDGE('',*,*,#3409,.T.);
#4467=ORIENTED_EDGE('',*,*,#3410,.T.);
#4468=ORIENTED_EDGE('',*,*,#3409,.F.);
#4469=ORIENTED_EDGE('',*,*,#3410,.F.);
#4470=ORIENTED_EDGE('',*,*,#3411,.T.);
#4471=ORIENTED_EDGE('',*,*,#3411,.F.);
#4472=ORIENTED_EDGE('',*,*,#3412,.T.);
#4473=ORIENTED_EDGE('',*,*,#3413,.T.);
#4474=ORIENTED_EDGE('',*,*,#3412,.F.);
#4475=ORIENTED_EDGE('',*,*,#3413,.F.);
#4476=ORIENTED_EDGE('',*,*,#3414,.T.);
#4477=ORIENTED_EDGE('',*,*,#3414,.F.);
#4478=ORIENTED_EDGE('',*,*,#3415,.T.);
#4479=ORIENTED_EDGE('',*,*,#3416,.T.);
#4480=ORIENTED_EDGE('',*,*,#3415,.F.);
#4481=ORIENTED_EDGE('',*,*,#3417,.T.);
#4482=ORIENTED_EDGE('',*,*,#3416,.F.);
#4483=ORIENTED_EDGE('',*,*,#3417,.F.);
#4484=ORIENTED_EDGE('',*,*,#3418,.T.);
#4485=ORIENTED_EDGE('',*,*,#3419,.F.);
#4486=ORIENTED_EDGE('',*,*,#3418,.F.);
#4487=ORIENTED_EDGE('',*,*,#3420,.F.);
#4488=ORIENTED_EDGE('',*,*,#3421,.T.);
#4489=ORIENTED_EDGE('',*,*,#3422,.T.);
#4490=ORIENTED_EDGE('',*,*,#3421,.F.);
#4491=ORIENTED_EDGE('',*,*,#3423,.T.);
#4492=ORIENTED_EDGE('',*,*,#3422,.F.);
#4493=ORIENTED_EDGE('',*,*,#3423,.F.);
#4494=ORIENTED_EDGE('',*,*,#3424,.T.);
#4495=ORIENTED_EDGE('',*,*,#3425,.T.);
#4496=ORIENTED_EDGE('',*,*,#3424,.F.);
#4497=ORIENTED_EDGE('',*,*,#3425,.F.);
#4498=ORIENTED_EDGE('',*,*,#3426,.T.);
#4499=ORIENTED_EDGE('',*,*,#3426,.F.);
#4500=ORIENTED_EDGE('',*,*,#3427,.T.);
#4501=ORIENTED_EDGE('',*,*,#3428,.T.);
#4502=ORIENTED_EDGE('',*,*,#3427,.F.);
#4503=ORIENTED_EDGE('',*,*,#3428,.F.);
#4504=ORIENTED_EDGE('',*,*,#3429,.T.);
#4505=ORIENTED_EDGE('',*,*,#3429,.F.);
#4506=ORIENTED_EDGE('',*,*,#3430,.T.);
#4507=ORIENTED_EDGE('',*,*,#3431,.F.);
#4508=ORIENTED_EDGE('',*,*,#3430,.F.);
#4509=ORIENTED_EDGE('',*,*,#3432,.F.);
#4510=ORIENTED_EDGE('',*,*,#3433,.T.);
#4511=ORIENTED_EDGE('',*,*,#3434,.T.);
#4512=ORIENTED_EDGE('',*,*,#3433,.F.);
#4513=ORIENTED_EDGE('',*,*,#3435,.T.);
#4514=ORIENTED_EDGE('',*,*,#3434,.F.);
#4515=ORIENTED_EDGE('',*,*,#3435,.F.);
#4516=ORIENTED_EDGE('',*,*,#3436,.T.);
#4517=ORIENTED_EDGE('',*,*,#3437,.T.);
#4518=ORIENTED_EDGE('',*,*,#3436,.F.);
#4519=ORIENTED_EDGE('',*,*,#3438,.T.);
#4520=ORIENTED_EDGE('',*,*,#3437,.F.);
#4521=ORIENTED_EDGE('',*,*,#3438,.F.);
#4522=ORIENTED_EDGE('',*,*,#3439,.T.);
#4523=ORIENTED_EDGE('',*,*,#3440,.T.);
#4524=ORIENTED_EDGE('',*,*,#3439,.F.);
#4525=ORIENTED_EDGE('',*,*,#3440,.F.);
#4526=ORIENTED_EDGE('',*,*,#3441,.T.);
#4527=ORIENTED_EDGE('',*,*,#3441,.F.);
#4528=ORIENTED_EDGE('',*,*,#3442,.T.);
#4529=ORIENTED_EDGE('',*,*,#3443,.F.);
#4530=ORIENTED_EDGE('',*,*,#3442,.F.);
#4531=ORIENTED_EDGE('',*,*,#3444,.T.);
#4532=ORIENTED_EDGE('',*,*,#3445,.T.);
#4533=ORIENTED_EDGE('',*,*,#3446,.T.);
#4534=ORIENTED_EDGE('',*,*,#3445,.F.);
#4535=ORIENTED_EDGE('',*,*,#3447,.T.);
#4536=ORIENTED_EDGE('',*,*,#3444,.F.);
#4537=ORIENTED_EDGE('',*,*,#3448,.T.);
#4538=ORIENTED_EDGE('',*,*,#3449,.F.);
#4539=ORIENTED_EDGE('',*,*,#3450,.F.);
#4540=ORIENTED_EDGE('',*,*,#3448,.F.);
#4541=ORIENTED_EDGE('',*,*,#3447,.F.);
#4542=ORIENTED_EDGE('',*,*,#3451,.F.);
#4543=ORIENTED_EDGE('',*,*,#3452,.F.);
#4544=ORIENTED_EDGE('',*,*,#3453,.F.);
#4545=ORIENTED_EDGE('',*,*,#3454,.F.);
#4546=ORIENTED_EDGE('',*,*,#3455,.F.);
#4547=ORIENTED_EDGE('',*,*,#3456,.F.);
#4548=ORIENTED_EDGE('',*,*,#3457,.F.);
#4549=ORIENTED_EDGE('',*,*,#3458,.F.);
#4550=ORIENTED_EDGE('',*,*,#3446,.F.);
#4551=ORIENTED_EDGE('',*,*,#3449,.T.);
#4552=ORIENTED_EDGE('',*,*,#3450,.T.);
#4553=ORIENTED_EDGE('',*,*,#3459,.T.);
#4554=ORIENTED_EDGE('',*,*,#3460,.T.);
#4555=ORIENTED_EDGE('',*,*,#3459,.F.);
#4556=ORIENTED_EDGE('',*,*,#3460,.F.);
#4557=ORIENTED_EDGE('',*,*,#3405,.T.);
#4558=ORIENTED_EDGE('',*,*,#3461,.T.);
#4559=ORIENTED_EDGE('',*,*,#3451,.T.);
#4560=ORIENTED_EDGE('',*,*,#3462,.T.);
#4561=ORIENTED_EDGE('',*,*,#3463,.T.);
#4562=ORIENTED_EDGE('',*,*,#3461,.F.);
#4563=ORIENTED_EDGE('',*,*,#3464,.T.);
#4564=ORIENTED_EDGE('',*,*,#3465,.T.);
#4565=ORIENTED_EDGE('',*,*,#3452,.T.);
#4566=ORIENTED_EDGE('',*,*,#3466,.T.);
#4567=ORIENTED_EDGE('',*,*,#3453,.T.);
#4568=ORIENTED_EDGE('',*,*,#3465,.F.);
#4569=ORIENTED_EDGE('',*,*,#3467,.T.);
#4570=ORIENTED_EDGE('',*,*,#3466,.F.);
#4571=ORIENTED_EDGE('',*,*,#3468,.T.);
#4572=ORIENTED_EDGE('',*,*,#3469,.T.);
#4573=ORIENTED_EDGE('',*,*,#3454,.T.);
#4574=ORIENTED_EDGE('',*,*,#3469,.F.);
#4575=ORIENTED_EDGE('',*,*,#3470,.T.);
#4576=ORIENTED_EDGE('',*,*,#3471,.T.);
#4577=ORIENTED_EDGE('',*,*,#3455,.T.);
#4578=ORIENTED_EDGE('',*,*,#3471,.F.);
#4579=ORIENTED_EDGE('',*,*,#3472,.T.);
#4580=ORIENTED_EDGE('',*,*,#3473,.T.);
#4581=ORIENTED_EDGE('',*,*,#3456,.T.);
#4582=ORIENTED_EDGE('',*,*,#3473,.F.);
#4583=ORIENTED_EDGE('',*,*,#3474,.T.);
#4584=ORIENTED_EDGE('',*,*,#3475,.T.);
#4585=ORIENTED_EDGE('',*,*,#3457,.T.);
#4586=ORIENTED_EDGE('',*,*,#3475,.F.);
#4587=ORIENTED_EDGE('',*,*,#3476,.T.);
#4588=ORIENTED_EDGE('',*,*,#3462,.F.);
#4589=ORIENTED_EDGE('',*,*,#3458,.T.);
#4590=ORIENTED_EDGE('',*,*,#3468,.F.);
#4591=ORIENTED_EDGE('',*,*,#3477,.T.);
#4592=ORIENTED_EDGE('',*,*,#3478,.F.);
#4593=ORIENTED_EDGE('',*,*,#3479,.T.);
#4594=ORIENTED_EDGE('',*,*,#3467,.F.);
#4595=ORIENTED_EDGE('',*,*,#3480,.F.);
#4596=ORIENTED_EDGE('',*,*,#3481,.F.);
#4597=ORIENTED_EDGE('',*,*,#3477,.F.);
#4598=ORIENTED_EDGE('',*,*,#3420,.T.);
#4599=ORIENTED_EDGE('',*,*,#3464,.F.);
#4600=ORIENTED_EDGE('',*,*,#3482,.T.);
#4601=ORIENTED_EDGE('',*,*,#3483,.F.);
#4602=ORIENTED_EDGE('',*,*,#3480,.T.);
#4603=ORIENTED_EDGE('',*,*,#3463,.F.);
#4604=ORIENTED_EDGE('',*,*,#3484,.F.);
#4605=ORIENTED_EDGE('',*,*,#3485,.F.);
#4606=ORIENTED_EDGE('',*,*,#3482,.F.);
#4607=ORIENTED_EDGE('',*,*,#3486,.T.);
#4608=ORIENTED_EDGE('',*,*,#3478,.T.);
#4609=ORIENTED_EDGE('',*,*,#3487,.T.);
#4610=ORIENTED_EDGE('',*,*,#3488,.T.);
#4611=ORIENTED_EDGE('',*,*,#3489,.T.);
#4612=ORIENTED_EDGE('',*,*,#3490,.T.);
#4613=ORIENTED_EDGE('',*,*,#3486,.F.);
#4614=ORIENTED_EDGE('',*,*,#3491,.T.);
#4615=ORIENTED_EDGE('',*,*,#3492,.T.);
#4616=ORIENTED_EDGE('',*,*,#3493,.T.);
#4617=ORIENTED_EDGE('',*,*,#3489,.F.);
#4618=ORIENTED_EDGE('',*,*,#3494,.T.);
#4619=ORIENTED_EDGE('',*,*,#3492,.F.);
#4620=ORIENTED_EDGE('',*,*,#3495,.T.);
#4621=ORIENTED_EDGE('',*,*,#3496,.T.);
#4622=ORIENTED_EDGE('',*,*,#3497,.T.);
#4623=ORIENTED_EDGE('',*,*,#3498,.T.);
#4624=ORIENTED_EDGE('',*,*,#3499,.T.);
#4625=ORIENTED_EDGE('',*,*,#3496,.F.);
#4626=ORIENTED_EDGE('',*,*,#3500,.T.);
#4627=ORIENTED_EDGE('',*,*,#3498,.F.);
#4628=ORIENTED_EDGE('',*,*,#3501,.T.);
#4629=ORIENTED_EDGE('',*,*,#3502,.T.);
#4630=ORIENTED_EDGE('',*,*,#3485,.T.);
#4631=ORIENTED_EDGE('',*,*,#3503,.T.);
#4632=ORIENTED_EDGE('',*,*,#3483,.T.);
#4633=ORIENTED_EDGE('',*,*,#3502,.F.);
#4634=ORIENTED_EDGE('',*,*,#3504,.T.);
#4635=ORIENTED_EDGE('',*,*,#3487,.F.);
#4636=ORIENTED_EDGE('',*,*,#3481,.T.);
#4637=ORIENTED_EDGE('',*,*,#3503,.F.);
#4638=ORIENTED_EDGE('',*,*,#3505,.T.);
#4639=ORIENTED_EDGE('',*,*,#3488,.F.);
#4640=ORIENTED_EDGE('',*,*,#3505,.F.);
#4641=ORIENTED_EDGE('',*,*,#3504,.F.);
#4642=ORIENTED_EDGE('',*,*,#3501,.F.);
#4643=ORIENTED_EDGE('',*,*,#3500,.F.);
#4644=ORIENTED_EDGE('',*,*,#3495,.F.);
#4645=ORIENTED_EDGE('',*,*,#3494,.F.);
#4646=ORIENTED_EDGE('',*,*,#3491,.F.);
#4647=ORIENTED_EDGE('',*,*,#3506,.F.);
#4648=ORIENTED_EDGE('',*,*,#3507,.F.);
#4649=ORIENTED_EDGE('',*,*,#3508,.F.);
#4650=ORIENTED_EDGE('',*,*,#3509,.F.);
#4651=ORIENTED_EDGE('',*,*,#3510,.F.);
#4652=ORIENTED_EDGE('',*,*,#3511,.F.);
#4653=ORIENTED_EDGE('',*,*,#3512,.F.);
#4654=ORIENTED_EDGE('',*,*,#3513,.F.);
#4655=ORIENTED_EDGE('',*,*,#3514,.T.);
#4656=ORIENTED_EDGE('',*,*,#3515,.T.);
#4657=ORIENTED_EDGE('',*,*,#3516,.T.);
#4658=ORIENTED_EDGE('',*,*,#3506,.T.);
#4659=ORIENTED_EDGE('',*,*,#3514,.F.);
#4660=ORIENTED_EDGE('',*,*,#3513,.T.);
#4661=ORIENTED_EDGE('',*,*,#3517,.T.);
#4662=ORIENTED_EDGE('',*,*,#3518,.T.);
#4663=ORIENTED_EDGE('',*,*,#3519,.T.);
#4664=ORIENTED_EDGE('',*,*,#3520,.T.);
#4665=ORIENTED_EDGE('',*,*,#3517,.F.);
#4666=ORIENTED_EDGE('',*,*,#3512,.T.);
#4667=ORIENTED_EDGE('',*,*,#3519,.F.);
#4668=ORIENTED_EDGE('',*,*,#3511,.T.);
#4669=ORIENTED_EDGE('',*,*,#3521,.T.);
#4670=ORIENTED_EDGE('',*,*,#3522,.T.);
#4671=ORIENTED_EDGE('',*,*,#3523,.T.);
#4672=ORIENTED_EDGE('',*,*,#3524,.T.);
#4673=ORIENTED_EDGE('',*,*,#3521,.F.);
#4674=ORIENTED_EDGE('',*,*,#3510,.T.);
#4675=ORIENTED_EDGE('',*,*,#3523,.F.);
#4676=ORIENTED_EDGE('',*,*,#3509,.T.);
#4677=ORIENTED_EDGE('',*,*,#3525,.T.);
#4678=ORIENTED_EDGE('',*,*,#3526,.T.);
#4679=ORIENTED_EDGE('',*,*,#3527,.T.);
#4680=ORIENTED_EDGE('',*,*,#3528,.T.);
#4681=ORIENTED_EDGE('',*,*,#3525,.F.);
#4682=ORIENTED_EDGE('',*,*,#3508,.T.);
#4683=ORIENTED_EDGE('',*,*,#3527,.F.);
#4684=ORIENTED_EDGE('',*,*,#3507,.T.);
#4685=ORIENTED_EDGE('',*,*,#3516,.F.);
#4686=ORIENTED_EDGE('',*,*,#3529,.T.);
#4687=ORIENTED_EDGE('',*,*,#3526,.F.);
#4688=ORIENTED_EDGE('',*,*,#3530,.F.);
#4689=ORIENTED_EDGE('',*,*,#3531,.F.);
#4690=ORIENTED_EDGE('',*,*,#3532,.F.);
#4691=ORIENTED_EDGE('',*,*,#3432,.T.);
#4692=ORIENTED_EDGE('',*,*,#3528,.F.);
#4693=ORIENTED_EDGE('',*,*,#3533,.T.);
#4694=ORIENTED_EDGE('',*,*,#3534,.F.);
#4695=ORIENTED_EDGE('',*,*,#3530,.T.);
#4696=ORIENTED_EDGE('',*,*,#3529,.F.);
#4697=ORIENTED_EDGE('',*,*,#3535,.F.);
#4698=ORIENTED_EDGE('',*,*,#3536,.F.);
#4699=ORIENTED_EDGE('',*,*,#3533,.F.);
#4700=ORIENTED_EDGE('',*,*,#3515,.F.);
#4701=ORIENTED_EDGE('',*,*,#3537,.T.);
#4702=ORIENTED_EDGE('',*,*,#3538,.F.);
#4703=ORIENTED_EDGE('',*,*,#3535,.T.);
#4704=ORIENTED_EDGE('',*,*,#3538,.T.);
#4705=ORIENTED_EDGE('',*,*,#3539,.F.);
#4706=ORIENTED_EDGE('',*,*,#3540,.T.);
#4707=ORIENTED_EDGE('',*,*,#3541,.F.);
#4708=ORIENTED_EDGE('',*,*,#3542,.T.);
#4709=ORIENTED_EDGE('',*,*,#3531,.T.);
#4710=ORIENTED_EDGE('',*,*,#3534,.T.);
#4711=ORIENTED_EDGE('',*,*,#3536,.T.);
#4712=ORIENTED_EDGE('',*,*,#3419,.T.);
#4713=ORIENTED_EDGE('',*,*,#3518,.F.);
#4714=ORIENTED_EDGE('',*,*,#3543,.F.);
#4715=ORIENTED_EDGE('',*,*,#3539,.T.);
#4716=ORIENTED_EDGE('',*,*,#3537,.F.);
#4717=ORIENTED_EDGE('',*,*,#3431,.T.);
#4718=ORIENTED_EDGE('',*,*,#3520,.F.);
#4719=ORIENTED_EDGE('',*,*,#3544,.T.);
#4720=ORIENTED_EDGE('',*,*,#3540,.F.);
#4721=ORIENTED_EDGE('',*,*,#3543,.T.);
#4722=ORIENTED_EDGE('',*,*,#3524,.F.);
#4723=ORIENTED_EDGE('',*,*,#3532,.T.);
#4724=ORIENTED_EDGE('',*,*,#3542,.F.);
#4725=ORIENTED_EDGE('',*,*,#3545,.T.);
#4726=ORIENTED_EDGE('',*,*,#3522,.F.);
#4727=ORIENTED_EDGE('',*,*,#3545,.F.);
#4728=ORIENTED_EDGE('',*,*,#3541,.T.);
#4729=ORIENTED_EDGE('',*,*,#3544,.F.);
#4730=ORIENTED_EDGE('',*,*,#3472,.F.);
#4731=ORIENTED_EDGE('',*,*,#3546,.T.);
#4732=ORIENTED_EDGE('',*,*,#3493,.F.);
#4733=ORIENTED_EDGE('',*,*,#3547,.T.);
#4734=ORIENTED_EDGE('',*,*,#3474,.F.);
#4735=ORIENTED_EDGE('',*,*,#3547,.F.);
#4736=ORIENTED_EDGE('',*,*,#3497,.F.);
#4737=ORIENTED_EDGE('',*,*,#3548,.F.);
#4738=ORIENTED_EDGE('',*,*,#3443,.T.);
#4739=ORIENTED_EDGE('',*,*,#3476,.F.);
#4740=ORIENTED_EDGE('',*,*,#3548,.T.);
#4741=ORIENTED_EDGE('',*,*,#3499,.F.);
#4742=ORIENTED_EDGE('',*,*,#3484,.T.);
#4743=ORIENTED_EDGE('',*,*,#3470,.F.);
#4744=ORIENTED_EDGE('',*,*,#3479,.F.);
#4745=ORIENTED_EDGE('',*,*,#3490,.F.);
#4746=ORIENTED_EDGE('',*,*,#3546,.F.);
#4747=ORIENTED_EDGE('',*,*,#3549,.F.);
#4748=ORIENTED_EDGE('',*,*,#3550,.T.);
#4749=ORIENTED_EDGE('',*,*,#3551,.T.);
#4750=ORIENTED_EDGE('',*,*,#3552,.T.);
#4751=ORIENTED_EDGE('',*,*,#3553,.F.);
#4752=ORIENTED_EDGE('',*,*,#3554,.F.);
#4753=ORIENTED_EDGE('',*,*,#3555,.F.);
#4754=ORIENTED_EDGE('',*,*,#3556,.T.);
#4755=ORIENTED_EDGE('',*,*,#3557,.T.);
#4756=ORIENTED_EDGE('',*,*,#3556,.F.);
#4757=ORIENTED_EDGE('',*,*,#3557,.F.);
#4758=ORIENTED_EDGE('',*,*,#3558,.T.);
#4759=ORIENTED_EDGE('',*,*,#3559,.F.);
#4760=ORIENTED_EDGE('',*,*,#3560,.F.);
#4761=ORIENTED_EDGE('',*,*,#3561,.F.);
#4762=ORIENTED_EDGE('',*,*,#3558,.F.);
#4763=ORIENTED_EDGE('',*,*,#3562,.F.);
#4764=ORIENTED_EDGE('',*,*,#3563,.T.);
#4765=ORIENTED_EDGE('',*,*,#3564,.T.);
#4766=ORIENTED_EDGE('',*,*,#3563,.F.);
#4767=ORIENTED_EDGE('',*,*,#3565,.F.);
#4768=ORIENTED_EDGE('',*,*,#3564,.F.);
#4769=ORIENTED_EDGE('',*,*,#3566,.T.);
#4770=ORIENTED_EDGE('',*,*,#3567,.F.);
#4771=ORIENTED_EDGE('',*,*,#3568,.F.);
#4772=ORIENTED_EDGE('',*,*,#3566,.F.);
#4773=ORIENTED_EDGE('',*,*,#3569,.T.);
#4774=ORIENTED_EDGE('',*,*,#3570,.T.);
#4775=ORIENTED_EDGE('',*,*,#3571,.T.);
#4776=ORIENTED_EDGE('',*,*,#3572,.T.);
#4777=ORIENTED_EDGE('',*,*,#3570,.F.);
#4778=ORIENTED_EDGE('',*,*,#3573,.F.);
#4779=ORIENTED_EDGE('',*,*,#3574,.F.);
#4780=ORIENTED_EDGE('',*,*,#3575,.T.);
#4781=ORIENTED_EDGE('',*,*,#3559,.T.);
#4782=ORIENTED_EDGE('',*,*,#3561,.T.);
#4783=ORIENTED_EDGE('',*,*,#3576,.T.);
#4784=ORIENTED_EDGE('',*,*,#3571,.F.);
#4785=ORIENTED_EDGE('',*,*,#3572,.F.);
#4786=ORIENTED_EDGE('',*,*,#3576,.F.);
#4787=ORIENTED_EDGE('',*,*,#3560,.T.);
#4788=ORIENTED_EDGE('',*,*,#3575,.F.);
#4789=ORIENTED_EDGE('',*,*,#3567,.T.);
#4790=ORIENTED_EDGE('',*,*,#3568,.T.);
#4791=ORIENTED_EDGE('',*,*,#3577,.F.);
#4792=ORIENTED_EDGE('',*,*,#3578,.T.);
#4793=ORIENTED_EDGE('',*,*,#3579,.T.);
#4794=ORIENTED_EDGE('',*,*,#3580,.F.);
#4795=ORIENTED_EDGE('',*,*,#3581,.T.);
#4796=ORIENTED_EDGE('',*,*,#3582,.T.);
#4797=ORIENTED_EDGE('',*,*,#3583,.F.);
#4798=ORIENTED_EDGE('',*,*,#3584,.T.);
#4799=ORIENTED_EDGE('',*,*,#3585,.T.);
#4800=ORIENTED_EDGE('',*,*,#3586,.F.);
#4801=ORIENTED_EDGE('',*,*,#3587,.T.);
#4802=ORIENTED_EDGE('',*,*,#3588,.T.);
#4803=ORIENTED_EDGE('',*,*,#3589,.F.);
#4804=ORIENTED_EDGE('',*,*,#3590,.T.);
#4805=ORIENTED_EDGE('',*,*,#3591,.T.);
#4806=ORIENTED_EDGE('',*,*,#3592,.F.);
#4807=ORIENTED_EDGE('',*,*,#3593,.T.);
#4808=ORIENTED_EDGE('',*,*,#3594,.T.);
#4809=ORIENTED_EDGE('',*,*,#3595,.F.);
#4810=ORIENTED_EDGE('',*,*,#3596,.T.);
#4811=ORIENTED_EDGE('',*,*,#3597,.T.);
#4812=ORIENTED_EDGE('',*,*,#3598,.F.);
#4813=ORIENTED_EDGE('',*,*,#3599,.T.);
#4814=ORIENTED_EDGE('',*,*,#3600,.T.);
#4815=ORIENTED_EDGE('',*,*,#3601,.F.);
#4816=ORIENTED_EDGE('',*,*,#3602,.T.);
#4817=ORIENTED_EDGE('',*,*,#3603,.T.);
#4818=ORIENTED_EDGE('',*,*,#3551,.F.);
#4819=ORIENTED_EDGE('',*,*,#3604,.T.);
#4820=ORIENTED_EDGE('',*,*,#3605,.T.);
#4821=ORIENTED_EDGE('',*,*,#3606,.F.);
#4822=ORIENTED_EDGE('',*,*,#3607,.T.);
#4823=ORIENTED_EDGE('',*,*,#3608,.T.);
#4824=ORIENTED_EDGE('',*,*,#3609,.F.);
#4825=ORIENTED_EDGE('',*,*,#3610,.T.);
#4826=ORIENTED_EDGE('',*,*,#3611,.T.);
#4827=ORIENTED_EDGE('',*,*,#3612,.F.);
#4828=ORIENTED_EDGE('',*,*,#3613,.T.);
#4829=ORIENTED_EDGE('',*,*,#3614,.T.);
#4830=ORIENTED_EDGE('',*,*,#3615,.F.);
#4831=ORIENTED_EDGE('',*,*,#3616,.T.);
#4832=ORIENTED_EDGE('',*,*,#3617,.T.);
#4833=ORIENTED_EDGE('',*,*,#3618,.F.);
#4834=ORIENTED_EDGE('',*,*,#3619,.T.);
#4835=ORIENTED_EDGE('',*,*,#3620,.T.);
#4836=ORIENTED_EDGE('',*,*,#3621,.F.);
#4837=ORIENTED_EDGE('',*,*,#3622,.T.);
#4838=ORIENTED_EDGE('',*,*,#3623,.T.);
#4839=ORIENTED_EDGE('',*,*,#3624,.F.);
#4840=ORIENTED_EDGE('',*,*,#3625,.T.);
#4841=ORIENTED_EDGE('',*,*,#3626,.T.);
#4842=ORIENTED_EDGE('',*,*,#3627,.F.);
#4843=ORIENTED_EDGE('',*,*,#3628,.T.);
#4844=ORIENTED_EDGE('',*,*,#3629,.T.);
#4845=ORIENTED_EDGE('',*,*,#3630,.F.);
#4846=ORIENTED_EDGE('',*,*,#3631,.T.);
#4847=ORIENTED_EDGE('',*,*,#3632,.T.);
#4848=ORIENTED_EDGE('',*,*,#3633,.F.);
#4849=ORIENTED_EDGE('',*,*,#3634,.T.);
#4850=ORIENTED_EDGE('',*,*,#3635,.T.);
#4851=ORIENTED_EDGE('',*,*,#3569,.F.);
#4852=ORIENTED_EDGE('',*,*,#3573,.T.);
#4853=ORIENTED_EDGE('',*,*,#3574,.T.);
#4854=ORIENTED_EDGE('',*,*,#3636,.T.);
#4855=ORIENTED_EDGE('',*,*,#3637,.T.);
#4856=ORIENTED_EDGE('',*,*,#3636,.F.);
#4857=ORIENTED_EDGE('',*,*,#3638,.F.);
#4858=ORIENTED_EDGE('',*,*,#3637,.F.);
#4859=ORIENTED_EDGE('',*,*,#3638,.T.);
#4860=ORIENTED_EDGE('',*,*,#3639,.T.);
#4861=ORIENTED_EDGE('',*,*,#3640,.T.);
#4862=ORIENTED_EDGE('',*,*,#3641,.T.);
#4863=ORIENTED_EDGE('',*,*,#3639,.F.);
#4864=ORIENTED_EDGE('',*,*,#3640,.F.);
#4865=ORIENTED_EDGE('',*,*,#3641,.F.);
#4866=ORIENTED_EDGE('',*,*,#3642,.T.);
#4867=ORIENTED_EDGE('',*,*,#3554,.T.);
#4868=ORIENTED_EDGE('',*,*,#3643,.T.);
#4869=ORIENTED_EDGE('',*,*,#3644,.T.);
#4870=ORIENTED_EDGE('',*,*,#3643,.F.);
#4871=ORIENTED_EDGE('',*,*,#3553,.T.);
#4872=ORIENTED_EDGE('',*,*,#3555,.T.);
#4873=ORIENTED_EDGE('',*,*,#3642,.F.);
#4874=ORIENTED_EDGE('',*,*,#3562,.T.);
#4875=ORIENTED_EDGE('',*,*,#3565,.T.);
#4876=ORIENTED_EDGE('',*,*,#3645,.F.);
#4877=ORIENTED_EDGE('',*,*,#3646,.F.);
#4878=ORIENTED_EDGE('',*,*,#3647,.F.);
#4879=ORIENTED_EDGE('',*,*,#3648,.F.);
#4880=ORIENTED_EDGE('',*,*,#3649,.F.);
#4881=ORIENTED_EDGE('',*,*,#3650,.F.);
#4882=ORIENTED_EDGE('',*,*,#3651,.F.);
#4883=ORIENTED_EDGE('',*,*,#3652,.F.);
#4884=ORIENTED_EDGE('',*,*,#3653,.F.);
#4885=ORIENTED_EDGE('',*,*,#3654,.F.);
#4886=ORIENTED_EDGE('',*,*,#3655,.F.);
#4887=ORIENTED_EDGE('',*,*,#3656,.F.);
#4888=ORIENTED_EDGE('',*,*,#3657,.F.);
#4889=ORIENTED_EDGE('',*,*,#3658,.F.);
#4890=ORIENTED_EDGE('',*,*,#3659,.F.);
#4891=ORIENTED_EDGE('',*,*,#3660,.F.);
#4892=ORIENTED_EDGE('',*,*,#3661,.F.);
#4893=ORIENTED_EDGE('',*,*,#3662,.F.);
#4894=ORIENTED_EDGE('',*,*,#3663,.F.);
#4895=ORIENTED_EDGE('',*,*,#3664,.F.);
#4896=ORIENTED_EDGE('',*,*,#3665,.F.);
#4897=ORIENTED_EDGE('',*,*,#3666,.F.);
#4898=ORIENTED_EDGE('',*,*,#3667,.F.);
#4899=ORIENTED_EDGE('',*,*,#3668,.F.);
#4900=ORIENTED_EDGE('',*,*,#3669,.F.);
#4901=ORIENTED_EDGE('',*,*,#3670,.F.);
#4902=ORIENTED_EDGE('',*,*,#3671,.F.);
#4903=ORIENTED_EDGE('',*,*,#3672,.F.);
#4904=ORIENTED_EDGE('',*,*,#3673,.F.);
#4905=ORIENTED_EDGE('',*,*,#3674,.F.);
#4906=ORIENTED_EDGE('',*,*,#3675,.F.);
#4907=ORIENTED_EDGE('',*,*,#3676,.F.);
#4908=ORIENTED_EDGE('',*,*,#3677,.F.);
#4909=ORIENTED_EDGE('',*,*,#3678,.F.);
#4910=ORIENTED_EDGE('',*,*,#3679,.F.);
#4911=ORIENTED_EDGE('',*,*,#3680,.F.);
#4912=ORIENTED_EDGE('',*,*,#3681,.F.);
#4913=ORIENTED_EDGE('',*,*,#3682,.F.);
#4914=ORIENTED_EDGE('',*,*,#3683,.F.);
#4915=ORIENTED_EDGE('',*,*,#3684,.F.);
#4916=ORIENTED_EDGE('',*,*,#3685,.F.);
#4917=ORIENTED_EDGE('',*,*,#3686,.F.);
#4918=ORIENTED_EDGE('',*,*,#3687,.F.);
#4919=ORIENTED_EDGE('',*,*,#3688,.F.);
#4920=ORIENTED_EDGE('',*,*,#3689,.F.);
#4921=ORIENTED_EDGE('',*,*,#3690,.F.);
#4922=ORIENTED_EDGE('',*,*,#3691,.F.);
#4923=ORIENTED_EDGE('',*,*,#3692,.F.);
#4924=ORIENTED_EDGE('',*,*,#3693,.F.);
#4925=ORIENTED_EDGE('',*,*,#3694,.F.);
#4926=ORIENTED_EDGE('',*,*,#3695,.F.);
#4927=ORIENTED_EDGE('',*,*,#3696,.F.);
#4928=ORIENTED_EDGE('',*,*,#3697,.F.);
#4929=ORIENTED_EDGE('',*,*,#3698,.F.);
#4930=ORIENTED_EDGE('',*,*,#3699,.F.);
#4931=ORIENTED_EDGE('',*,*,#3700,.F.);
#4932=ORIENTED_EDGE('',*,*,#3701,.F.);
#4933=ORIENTED_EDGE('',*,*,#3702,.F.);
#4934=ORIENTED_EDGE('',*,*,#3703,.T.);
#4935=ORIENTED_EDGE('',*,*,#3704,.F.);
#4936=ORIENTED_EDGE('',*,*,#3703,.F.);
#4937=ORIENTED_EDGE('',*,*,#3704,.T.);
#4938=ORIENTED_EDGE('',*,*,#3705,.T.);
#4939=ORIENTED_EDGE('',*,*,#3706,.F.);
#4940=ORIENTED_EDGE('',*,*,#3705,.F.);
#4941=ORIENTED_EDGE('',*,*,#3707,.F.);
#4942=ORIENTED_EDGE('',*,*,#3708,.F.);
#4943=ORIENTED_EDGE('',*,*,#3709,.F.);
#4944=ORIENTED_EDGE('',*,*,#3708,.T.);
#4945=ORIENTED_EDGE('',*,*,#3710,.F.);
#4946=ORIENTED_EDGE('',*,*,#3634,.F.);
#4947=ORIENTED_EDGE('',*,*,#3711,.F.);
#4948=ORIENTED_EDGE('',*,*,#3712,.T.);
#4949=ORIENTED_EDGE('',*,*,#3700,.T.);
#4950=ORIENTED_EDGE('',*,*,#3713,.F.);
#4951=ORIENTED_EDGE('',*,*,#3578,.F.);
#4952=ORIENTED_EDGE('',*,*,#3714,.F.);
#4953=ORIENTED_EDGE('',*,*,#3715,.T.);
#4954=ORIENTED_EDGE('',*,*,#3697,.T.);
#4955=ORIENTED_EDGE('',*,*,#3716,.F.);
#4956=ORIENTED_EDGE('',*,*,#3581,.F.);
#4957=ORIENTED_EDGE('',*,*,#3717,.F.);
#4958=ORIENTED_EDGE('',*,*,#3718,.T.);
#4959=ORIENTED_EDGE('',*,*,#3694,.T.);
#4960=ORIENTED_EDGE('',*,*,#3719,.F.);
#4961=ORIENTED_EDGE('',*,*,#3584,.F.);
#4962=ORIENTED_EDGE('',*,*,#3720,.F.);
#4963=ORIENTED_EDGE('',*,*,#3721,.T.);
#4964=ORIENTED_EDGE('',*,*,#3691,.T.);
#4965=ORIENTED_EDGE('',*,*,#3722,.F.);
#4966=ORIENTED_EDGE('',*,*,#3587,.F.);
#4967=ORIENTED_EDGE('',*,*,#3723,.F.);
#4968=ORIENTED_EDGE('',*,*,#3724,.T.);
#4969=ORIENTED_EDGE('',*,*,#3688,.T.);
#4970=ORIENTED_EDGE('',*,*,#3725,.F.);
#4971=ORIENTED_EDGE('',*,*,#3590,.F.);
#4972=ORIENTED_EDGE('',*,*,#3726,.F.);
#4973=ORIENTED_EDGE('',*,*,#3727,.T.);
#4974=ORIENTED_EDGE('',*,*,#3685,.T.);
#4975=ORIENTED_EDGE('',*,*,#3728,.F.);
#4976=ORIENTED_EDGE('',*,*,#3593,.F.);
#4977=ORIENTED_EDGE('',*,*,#3729,.F.);
#4978=ORIENTED_EDGE('',*,*,#3730,.T.);
#4979=ORIENTED_EDGE('',*,*,#3682,.T.);
#4980=ORIENTED_EDGE('',*,*,#3731,.F.);
#4981=ORIENTED_EDGE('',*,*,#3596,.F.);
#4982=ORIENTED_EDGE('',*,*,#3732,.F.);
#4983=ORIENTED_EDGE('',*,*,#3733,.T.);
#4984=ORIENTED_EDGE('',*,*,#3679,.T.);
#4985=ORIENTED_EDGE('',*,*,#3734,.F.);
#4986=ORIENTED_EDGE('',*,*,#3599,.F.);
#4987=ORIENTED_EDGE('',*,*,#3735,.F.);
#4988=ORIENTED_EDGE('',*,*,#3736,.T.);
#4989=ORIENTED_EDGE('',*,*,#3676,.T.);
#4990=ORIENTED_EDGE('',*,*,#3737,.F.);
#4991=ORIENTED_EDGE('',*,*,#3602,.F.);
#4992=ORIENTED_EDGE('',*,*,#3738,.F.);
#4993=ORIENTED_EDGE('',*,*,#3739,.T.);
#4994=ORIENTED_EDGE('',*,*,#3673,.T.);
#4995=ORIENTED_EDGE('',*,*,#3740,.F.);
#4996=ORIENTED_EDGE('',*,*,#3604,.F.);
#4997=ORIENTED_EDGE('',*,*,#3550,.F.);
#4998=ORIENTED_EDGE('',*,*,#3741,.F.);
#4999=ORIENTED_EDGE('',*,*,#3742,.T.);
#5000=ORIENTED_EDGE('',*,*,#3670,.T.);
#5001=ORIENTED_EDGE('',*,*,#3743,.F.);
#5002=ORIENTED_EDGE('',*,*,#3607,.F.);
#5003=ORIENTED_EDGE('',*,*,#3744,.F.);
#5004=ORIENTED_EDGE('',*,*,#3745,.T.);
#5005=ORIENTED_EDGE('',*,*,#3667,.T.);
#5006=ORIENTED_EDGE('',*,*,#3746,.F.);
#5007=ORIENTED_EDGE('',*,*,#3610,.F.);
#5008=ORIENTED_EDGE('',*,*,#3747,.F.);
#5009=ORIENTED_EDGE('',*,*,#3748,.T.);
#5010=ORIENTED_EDGE('',*,*,#3664,.T.);
#5011=ORIENTED_EDGE('',*,*,#3749,.F.);
#5012=ORIENTED_EDGE('',*,*,#3613,.F.);
#5013=ORIENTED_EDGE('',*,*,#3750,.F.);
#5014=ORIENTED_EDGE('',*,*,#3751,.T.);
#5015=ORIENTED_EDGE('',*,*,#3661,.T.);
#5016=ORIENTED_EDGE('',*,*,#3752,.F.);
#5017=ORIENTED_EDGE('',*,*,#3616,.F.);
#5018=ORIENTED_EDGE('',*,*,#3753,.F.);
#5019=ORIENTED_EDGE('',*,*,#3754,.T.);
#5020=ORIENTED_EDGE('',*,*,#3658,.T.);
#5021=ORIENTED_EDGE('',*,*,#3755,.F.);
#5022=ORIENTED_EDGE('',*,*,#3619,.F.);
#5023=ORIENTED_EDGE('',*,*,#3756,.F.);
#5024=ORIENTED_EDGE('',*,*,#3757,.T.);
#5025=ORIENTED_EDGE('',*,*,#3655,.T.);
#5026=ORIENTED_EDGE('',*,*,#3758,.F.);
#5027=ORIENTED_EDGE('',*,*,#3622,.F.);
#5028=ORIENTED_EDGE('',*,*,#3759,.F.);
#5029=ORIENTED_EDGE('',*,*,#3760,.T.);
#5030=ORIENTED_EDGE('',*,*,#3652,.T.);
#5031=ORIENTED_EDGE('',*,*,#3761,.F.);
#5032=ORIENTED_EDGE('',*,*,#3625,.F.);
#5033=ORIENTED_EDGE('',*,*,#3762,.F.);
#5034=ORIENTED_EDGE('',*,*,#3763,.T.);
#5035=ORIENTED_EDGE('',*,*,#3649,.T.);
#5036=ORIENTED_EDGE('',*,*,#3764,.F.);
#5037=ORIENTED_EDGE('',*,*,#3628,.F.);
#5038=ORIENTED_EDGE('',*,*,#3765,.F.);
#5039=ORIENTED_EDGE('',*,*,#3766,.T.);
#5040=ORIENTED_EDGE('',*,*,#3646,.T.);
#5041=ORIENTED_EDGE('',*,*,#3767,.F.);
#5042=ORIENTED_EDGE('',*,*,#3631,.F.);
#5043=ORIENTED_EDGE('',*,*,#3768,.F.);
#5044=ORIENTED_EDGE('',*,*,#3769,.T.);
#5045=ORIENTED_EDGE('',*,*,#3707,.T.);
#5046=ORIENTED_EDGE('',*,*,#3770,.T.);
#5047=ORIENTED_EDGE('',*,*,#3771,.F.);
#5048=ORIENTED_EDGE('',*,*,#3635,.F.);
#5049=ORIENTED_EDGE('',*,*,#3710,.T.);
#5050=ORIENTED_EDGE('',*,*,#3709,.T.);
#5051=ORIENTED_EDGE('',*,*,#3712,.F.);
#5052=ORIENTED_EDGE('',*,*,#3772,.F.);
#5053=ORIENTED_EDGE('',*,*,#3770,.F.);
#5054=ORIENTED_EDGE('',*,*,#3702,.T.);
#5055=ORIENTED_EDGE('',*,*,#3773,.T.);
#5056=ORIENTED_EDGE('',*,*,#3774,.T.);
#5057=ORIENTED_EDGE('',*,*,#3741,.T.);
#5058=ORIENTED_EDGE('',*,*,#3549,.T.);
#5059=ORIENTED_EDGE('',*,*,#3775,.T.);
#5060=ORIENTED_EDGE('',*,*,#3776,.T.);
#5061=ORIENTED_EDGE('',*,*,#3738,.T.);
#5062=ORIENTED_EDGE('',*,*,#3601,.T.);
#5063=ORIENTED_EDGE('',*,*,#3777,.T.);
#5064=ORIENTED_EDGE('',*,*,#3778,.T.);
#5065=ORIENTED_EDGE('',*,*,#3735,.T.);
#5066=ORIENTED_EDGE('',*,*,#3598,.T.);
#5067=ORIENTED_EDGE('',*,*,#3779,.T.);
#5068=ORIENTED_EDGE('',*,*,#3780,.T.);
#5069=ORIENTED_EDGE('',*,*,#3732,.T.);
#5070=ORIENTED_EDGE('',*,*,#3595,.T.);
#5071=ORIENTED_EDGE('',*,*,#3781,.T.);
#5072=ORIENTED_EDGE('',*,*,#3782,.T.);
#5073=ORIENTED_EDGE('',*,*,#3729,.T.);
#5074=ORIENTED_EDGE('',*,*,#3592,.T.);
#5075=ORIENTED_EDGE('',*,*,#3783,.T.);
#5076=ORIENTED_EDGE('',*,*,#3784,.T.);
#5077=ORIENTED_EDGE('',*,*,#3726,.T.);
#5078=ORIENTED_EDGE('',*,*,#3589,.T.);
#5079=ORIENTED_EDGE('',*,*,#3785,.T.);
#5080=ORIENTED_EDGE('',*,*,#3786,.T.);
#5081=ORIENTED_EDGE('',*,*,#3723,.T.);
#5082=ORIENTED_EDGE('',*,*,#3586,.T.);
#5083=ORIENTED_EDGE('',*,*,#3787,.T.);
#5084=ORIENTED_EDGE('',*,*,#3788,.T.);
#5085=ORIENTED_EDGE('',*,*,#3720,.T.);
#5086=ORIENTED_EDGE('',*,*,#3583,.T.);
#5087=ORIENTED_EDGE('',*,*,#3789,.T.);
#5088=ORIENTED_EDGE('',*,*,#3790,.T.);
#5089=ORIENTED_EDGE('',*,*,#3717,.T.);
#5090=ORIENTED_EDGE('',*,*,#3580,.T.);
#5091=ORIENTED_EDGE('',*,*,#3791,.T.);
#5092=ORIENTED_EDGE('',*,*,#3792,.T.);
#5093=ORIENTED_EDGE('',*,*,#3714,.T.);
#5094=ORIENTED_EDGE('',*,*,#3577,.T.);
#5095=ORIENTED_EDGE('',*,*,#3771,.T.);
#5096=ORIENTED_EDGE('',*,*,#3772,.T.);
#5097=ORIENTED_EDGE('',*,*,#3711,.T.);
#5098=ORIENTED_EDGE('',*,*,#3633,.T.);
#5099=ORIENTED_EDGE('',*,*,#3793,.T.);
#5100=ORIENTED_EDGE('',*,*,#3794,.T.);
#5101=ORIENTED_EDGE('',*,*,#3768,.T.);
#5102=ORIENTED_EDGE('',*,*,#3630,.T.);
#5103=ORIENTED_EDGE('',*,*,#3795,.T.);
#5104=ORIENTED_EDGE('',*,*,#3796,.T.);
#5105=ORIENTED_EDGE('',*,*,#3765,.T.);
#5106=ORIENTED_EDGE('',*,*,#3627,.T.);
#5107=ORIENTED_EDGE('',*,*,#3797,.T.);
#5108=ORIENTED_EDGE('',*,*,#3798,.T.);
#5109=ORIENTED_EDGE('',*,*,#3762,.T.);
#5110=ORIENTED_EDGE('',*,*,#3624,.T.);
#5111=ORIENTED_EDGE('',*,*,#3799,.T.);
#5112=ORIENTED_EDGE('',*,*,#3800,.T.);
#5113=ORIENTED_EDGE('',*,*,#3759,.T.);
#5114=ORIENTED_EDGE('',*,*,#3621,.T.);
#5115=ORIENTED_EDGE('',*,*,#3801,.T.);
#5116=ORIENTED_EDGE('',*,*,#3802,.T.);
#5117=ORIENTED_EDGE('',*,*,#3756,.T.);
#5118=ORIENTED_EDGE('',*,*,#3618,.T.);
#5119=ORIENTED_EDGE('',*,*,#3803,.T.);
#5120=ORIENTED_EDGE('',*,*,#3804,.T.);
#5121=ORIENTED_EDGE('',*,*,#3753,.T.);
#5122=ORIENTED_EDGE('',*,*,#3615,.T.);
#5123=ORIENTED_EDGE('',*,*,#3805,.T.);
#5124=ORIENTED_EDGE('',*,*,#3806,.T.);
#5125=ORIENTED_EDGE('',*,*,#3750,.T.);
#5126=ORIENTED_EDGE('',*,*,#3612,.T.);
#5127=ORIENTED_EDGE('',*,*,#3807,.T.);
#5128=ORIENTED_EDGE('',*,*,#3808,.T.);
#5129=ORIENTED_EDGE('',*,*,#3747,.T.);
#5130=ORIENTED_EDGE('',*,*,#3609,.T.);
#5131=ORIENTED_EDGE('',*,*,#3809,.T.);
#5132=ORIENTED_EDGE('',*,*,#3810,.T.);
#5133=ORIENTED_EDGE('',*,*,#3744,.T.);
#5134=ORIENTED_EDGE('',*,*,#3606,.T.);
#5135=ORIENTED_EDGE('',*,*,#3811,.T.);
#5136=ORIENTED_EDGE('',*,*,#3812,.T.);
#5137=ORIENTED_EDGE('',*,*,#3773,.F.);
#5138=ORIENTED_EDGE('',*,*,#3699,.T.);
#5139=ORIENTED_EDGE('',*,*,#3813,.T.);
#5140=ORIENTED_EDGE('',*,*,#3791,.F.);
#5141=ORIENTED_EDGE('',*,*,#3579,.F.);
#5142=ORIENTED_EDGE('',*,*,#3713,.T.);
#5143=ORIENTED_EDGE('',*,*,#3701,.T.);
#5144=ORIENTED_EDGE('',*,*,#3715,.F.);
#5145=ORIENTED_EDGE('',*,*,#3792,.F.);
#5146=ORIENTED_EDGE('',*,*,#3813,.F.);
#5147=ORIENTED_EDGE('',*,*,#3696,.T.);
#5148=ORIENTED_EDGE('',*,*,#3814,.T.);
#5149=ORIENTED_EDGE('',*,*,#3789,.F.);
#5150=ORIENTED_EDGE('',*,*,#3582,.F.);
#5151=ORIENTED_EDGE('',*,*,#3716,.T.);
#5152=ORIENTED_EDGE('',*,*,#3698,.T.);
#5153=ORIENTED_EDGE('',*,*,#3718,.F.);
#5154=ORIENTED_EDGE('',*,*,#3790,.F.);
#5155=ORIENTED_EDGE('',*,*,#3814,.F.);
#5156=ORIENTED_EDGE('',*,*,#3693,.T.);
#5157=ORIENTED_EDGE('',*,*,#3815,.T.);
#5158=ORIENTED_EDGE('',*,*,#3787,.F.);
#5159=ORIENTED_EDGE('',*,*,#3585,.F.);
#5160=ORIENTED_EDGE('',*,*,#3719,.T.);
#5161=ORIENTED_EDGE('',*,*,#3695,.T.);
#5162=ORIENTED_EDGE('',*,*,#3721,.F.);
#5163=ORIENTED_EDGE('',*,*,#3788,.F.);
#5164=ORIENTED_EDGE('',*,*,#3815,.F.);
#5165=ORIENTED_EDGE('',*,*,#3690,.T.);
#5166=ORIENTED_EDGE('',*,*,#3816,.T.);
#5167=ORIENTED_EDGE('',*,*,#3785,.F.);
#5168=ORIENTED_EDGE('',*,*,#3588,.F.);
#5169=ORIENTED_EDGE('',*,*,#3722,.T.);
#5170=ORIENTED_EDGE('',*,*,#3692,.T.);
#5171=ORIENTED_EDGE('',*,*,#3724,.F.);
#5172=ORIENTED_EDGE('',*,*,#3786,.F.);
#5173=ORIENTED_EDGE('',*,*,#3816,.F.);
#5174=ORIENTED_EDGE('',*,*,#3687,.T.);
#5175=ORIENTED_EDGE('',*,*,#3817,.T.);
#5176=ORIENTED_EDGE('',*,*,#3783,.F.);
#5177=ORIENTED_EDGE('',*,*,#3591,.F.);
#5178=ORIENTED_EDGE('',*,*,#3725,.T.);
#5179=ORIENTED_EDGE('',*,*,#3689,.T.);
#5180=ORIENTED_EDGE('',*,*,#3727,.F.);
#5181=ORIENTED_EDGE('',*,*,#3784,.F.);
#5182=ORIENTED_EDGE('',*,*,#3817,.F.);
#5183=ORIENTED_EDGE('',*,*,#3684,.T.);
#5184=ORIENTED_EDGE('',*,*,#3818,.T.);
#5185=ORIENTED_EDGE('',*,*,#3781,.F.);
#5186=ORIENTED_EDGE('',*,*,#3594,.F.);
#5187=ORIENTED_EDGE('',*,*,#3728,.T.);
#5188=ORIENTED_EDGE('',*,*,#3686,.T.);
#5189=ORIENTED_EDGE('',*,*,#3730,.F.);
#5190=ORIENTED_EDGE('',*,*,#3782,.F.);
#5191=ORIENTED_EDGE('',*,*,#3818,.F.);
#5192=ORIENTED_EDGE('',*,*,#3681,.T.);
#5193=ORIENTED_EDGE('',*,*,#3819,.T.);
#5194=ORIENTED_EDGE('',*,*,#3779,.F.);
#5195=ORIENTED_EDGE('',*,*,#3597,.F.);
#5196=ORIENTED_EDGE('',*,*,#3731,.T.);
#5197=ORIENTED_EDGE('',*,*,#3683,.T.);
#5198=ORIENTED_EDGE('',*,*,#3733,.F.);
#5199=ORIENTED_EDGE('',*,*,#3780,.F.);
#5200=ORIENTED_EDGE('',*,*,#3819,.F.);
#5201=ORIENTED_EDGE('',*,*,#3678,.T.);
#5202=ORIENTED_EDGE('',*,*,#3820,.T.);
#5203=ORIENTED_EDGE('',*,*,#3777,.F.);
#5204=ORIENTED_EDGE('',*,*,#3600,.F.);
#5205=ORIENTED_EDGE('',*,*,#3734,.T.);
#5206=ORIENTED_EDGE('',*,*,#3680,.T.);
#5207=ORIENTED_EDGE('',*,*,#3736,.F.);
#5208=ORIENTED_EDGE('',*,*,#3778,.F.);
#5209=ORIENTED_EDGE('',*,*,#3820,.F.);
#5210=ORIENTED_EDGE('',*,*,#3675,.T.);
#5211=ORIENTED_EDGE('',*,*,#3821,.T.);
#5212=ORIENTED_EDGE('',*,*,#3775,.F.);
#5213=ORIENTED_EDGE('',*,*,#3552,.F.);
#5214=ORIENTED_EDGE('',*,*,#3603,.F.);
#5215=ORIENTED_EDGE('',*,*,#3737,.T.);
#5216=ORIENTED_EDGE('',*,*,#3677,.T.);
#5217=ORIENTED_EDGE('',*,*,#3739,.F.);
#5218=ORIENTED_EDGE('',*,*,#3776,.F.);
#5219=ORIENTED_EDGE('',*,*,#3821,.F.);
#5220=ORIENTED_EDGE('',*,*,#3672,.T.);
#5221=ORIENTED_EDGE('',*,*,#3822,.T.);
#5222=ORIENTED_EDGE('',*,*,#3811,.F.);
#5223=ORIENTED_EDGE('',*,*,#3605,.F.);
#5224=ORIENTED_EDGE('',*,*,#3740,.T.);
#5225=ORIENTED_EDGE('',*,*,#3674,.T.);
#5226=ORIENTED_EDGE('',*,*,#3742,.F.);
#5227=ORIENTED_EDGE('',*,*,#3774,.F.);
#5228=ORIENTED_EDGE('',*,*,#3812,.F.);
#5229=ORIENTED_EDGE('',*,*,#3822,.F.);
#5230=ORIENTED_EDGE('',*,*,#3669,.T.);
#5231=ORIENTED_EDGE('',*,*,#3823,.T.);
#5232=ORIENTED_EDGE('',*,*,#3809,.F.);
#5233=ORIENTED_EDGE('',*,*,#3608,.F.);
#5234=ORIENTED_EDGE('',*,*,#3743,.T.);
#5235=ORIENTED_EDGE('',*,*,#3671,.T.);
#5236=ORIENTED_EDGE('',*,*,#3745,.F.);
#5237=ORIENTED_EDGE('',*,*,#3810,.F.);
#5238=ORIENTED_EDGE('',*,*,#3823,.F.);
#5239=ORIENTED_EDGE('',*,*,#3666,.T.);
#5240=ORIENTED_EDGE('',*,*,#3824,.T.);
#5241=ORIENTED_EDGE('',*,*,#3807,.F.);
#5242=ORIENTED_EDGE('',*,*,#3611,.F.);
#5243=ORIENTED_EDGE('',*,*,#3746,.T.);
#5244=ORIENTED_EDGE('',*,*,#3668,.T.);
#5245=ORIENTED_EDGE('',*,*,#3748,.F.);
#5246=ORIENTED_EDGE('',*,*,#3808,.F.);
#5247=ORIENTED_EDGE('',*,*,#3824,.F.);
#5248=ORIENTED_EDGE('',*,*,#3663,.T.);
#5249=ORIENTED_EDGE('',*,*,#3825,.T.);
#5250=ORIENTED_EDGE('',*,*,#3805,.F.);
#5251=ORIENTED_EDGE('',*,*,#3614,.F.);
#5252=ORIENTED_EDGE('',*,*,#3749,.T.);
#5253=ORIENTED_EDGE('',*,*,#3665,.T.);
#5254=ORIENTED_EDGE('',*,*,#3751,.F.);
#5255=ORIENTED_EDGE('',*,*,#3806,.F.);
#5256=ORIENTED_EDGE('',*,*,#3825,.F.);
#5257=ORIENTED_EDGE('',*,*,#3660,.T.);
#5258=ORIENTED_EDGE('',*,*,#3826,.T.);
#5259=ORIENTED_EDGE('',*,*,#3803,.F.);
#5260=ORIENTED_EDGE('',*,*,#3617,.F.);
#5261=ORIENTED_EDGE('',*,*,#3752,.T.);
#5262=ORIENTED_EDGE('',*,*,#3662,.T.);
#5263=ORIENTED_EDGE('',*,*,#3754,.F.);
#5264=ORIENTED_EDGE('',*,*,#3804,.F.);
#5265=ORIENTED_EDGE('',*,*,#3826,.F.);
#5266=ORIENTED_EDGE('',*,*,#3657,.T.);
#5267=ORIENTED_EDGE('',*,*,#3827,.T.);
#5268=ORIENTED_EDGE('',*,*,#3801,.F.);
#5269=ORIENTED_EDGE('',*,*,#3620,.F.);
#5270=ORIENTED_EDGE('',*,*,#3755,.T.);
#5271=ORIENTED_EDGE('',*,*,#3659,.T.);
#5272=ORIENTED_EDGE('',*,*,#3757,.F.);
#5273=ORIENTED_EDGE('',*,*,#3802,.F.);
#5274=ORIENTED_EDGE('',*,*,#3827,.F.);
#5275=ORIENTED_EDGE('',*,*,#3654,.T.);
#5276=ORIENTED_EDGE('',*,*,#3828,.T.);
#5277=ORIENTED_EDGE('',*,*,#3799,.F.);
#5278=ORIENTED_EDGE('',*,*,#3623,.F.);
#5279=ORIENTED_EDGE('',*,*,#3758,.T.);
#5280=ORIENTED_EDGE('',*,*,#3656,.T.);
#5281=ORIENTED_EDGE('',*,*,#3760,.F.);
#5282=ORIENTED_EDGE('',*,*,#3800,.F.);
#5283=ORIENTED_EDGE('',*,*,#3828,.F.);
#5284=ORIENTED_EDGE('',*,*,#3651,.T.);
#5285=ORIENTED_EDGE('',*,*,#3829,.T.);
#5286=ORIENTED_EDGE('',*,*,#3797,.F.);
#5287=ORIENTED_EDGE('',*,*,#3626,.F.);
#5288=ORIENTED_EDGE('',*,*,#3761,.T.);
#5289=ORIENTED_EDGE('',*,*,#3653,.T.);
#5290=ORIENTED_EDGE('',*,*,#3763,.F.);
#5291=ORIENTED_EDGE('',*,*,#3798,.F.);
#5292=ORIENTED_EDGE('',*,*,#3829,.F.);
#5293=ORIENTED_EDGE('',*,*,#3648,.T.);
#5294=ORIENTED_EDGE('',*,*,#3830,.T.);
#5295=ORIENTED_EDGE('',*,*,#3795,.F.);
#5296=ORIENTED_EDGE('',*,*,#3629,.F.);
#5297=ORIENTED_EDGE('',*,*,#3764,.T.);
#5298=ORIENTED_EDGE('',*,*,#3650,.T.);
#5299=ORIENTED_EDGE('',*,*,#3766,.F.);
#5300=ORIENTED_EDGE('',*,*,#3796,.F.);
#5301=ORIENTED_EDGE('',*,*,#3830,.F.);
#5302=ORIENTED_EDGE('',*,*,#3645,.T.);
#5303=ORIENTED_EDGE('',*,*,#3831,.T.);
#5304=ORIENTED_EDGE('',*,*,#3793,.F.);
#5305=ORIENTED_EDGE('',*,*,#3632,.F.);
#5306=ORIENTED_EDGE('',*,*,#3767,.T.);
#5307=ORIENTED_EDGE('',*,*,#3647,.T.);
#5308=ORIENTED_EDGE('',*,*,#3769,.F.);
#5309=ORIENTED_EDGE('',*,*,#3794,.F.);
#5310=ORIENTED_EDGE('',*,*,#3831,.F.);
#5311=ORIENTED_EDGE('',*,*,#3706,.T.);
#5312=ORIENTED_EDGE('',*,*,#3644,.F.);
#5313=ORIENTED_EDGE('',*,*,#3832,.F.);
#5314=ORIENTED_EDGE('',*,*,#3833,.F.);
#5315=ORIENTED_EDGE('',*,*,#3834,.F.);
#5316=ORIENTED_EDGE('',*,*,#3835,.T.);
#5317=ORIENTED_EDGE('',*,*,#3836,.T.);
#5318=ORIENTED_EDGE('',*,*,#3835,.F.);
#5319=ORIENTED_EDGE('',*,*,#3836,.F.);
#5320=ORIENTED_EDGE('',*,*,#3837,.T.);
#5321=ORIENTED_EDGE('',*,*,#3838,.F.);
#5322=ORIENTED_EDGE('',*,*,#3839,.F.);
#5323=ORIENTED_EDGE('',*,*,#3840,.F.);
#5324=ORIENTED_EDGE('',*,*,#3837,.F.);
#5325=ORIENTED_EDGE('',*,*,#3841,.F.);
#5326=ORIENTED_EDGE('',*,*,#3842,.T.);
#5327=ORIENTED_EDGE('',*,*,#3843,.T.);
#5328=ORIENTED_EDGE('',*,*,#3842,.F.);
#5329=ORIENTED_EDGE('',*,*,#3844,.F.);
#5330=ORIENTED_EDGE('',*,*,#3843,.F.);
#5331=ORIENTED_EDGE('',*,*,#3845,.T.);
#5332=ORIENTED_EDGE('',*,*,#3846,.F.);
#5333=ORIENTED_EDGE('',*,*,#3847,.F.);
#5334=ORIENTED_EDGE('',*,*,#3845,.F.);
#5335=ORIENTED_EDGE('',*,*,#3848,.T.);
#5336=ORIENTED_EDGE('',*,*,#3849,.T.);
#5337=ORIENTED_EDGE('',*,*,#3850,.T.);
#5338=ORIENTED_EDGE('',*,*,#3851,.T.);
#5339=ORIENTED_EDGE('',*,*,#3849,.F.);
#5340=ORIENTED_EDGE('',*,*,#3852,.F.);
#5341=ORIENTED_EDGE('',*,*,#3853,.F.);
#5342=ORIENTED_EDGE('',*,*,#3854,.T.);
#5343=ORIENTED_EDGE('',*,*,#3838,.T.);
#5344=ORIENTED_EDGE('',*,*,#3840,.T.);
#5345=ORIENTED_EDGE('',*,*,#3855,.T.);
#5346=ORIENTED_EDGE('',*,*,#3850,.F.);
#5347=ORIENTED_EDGE('',*,*,#3851,.F.);
#5348=ORIENTED_EDGE('',*,*,#3855,.F.);
#5349=ORIENTED_EDGE('',*,*,#3839,.T.);
#5350=ORIENTED_EDGE('',*,*,#3854,.F.);
#5351=ORIENTED_EDGE('',*,*,#3846,.T.);
#5352=ORIENTED_EDGE('',*,*,#3847,.T.);
#5353=ORIENTED_EDGE('',*,*,#3856,.F.);
#5354=ORIENTED_EDGE('',*,*,#3857,.T.);
#5355=ORIENTED_EDGE('',*,*,#3858,.T.);
#5356=ORIENTED_EDGE('',*,*,#3859,.F.);
#5357=ORIENTED_EDGE('',*,*,#3860,.T.);
#5358=ORIENTED_EDGE('',*,*,#3861,.T.);
#5359=ORIENTED_EDGE('',*,*,#3862,.F.);
#5360=ORIENTED_EDGE('',*,*,#3863,.T.);
#5361=ORIENTED_EDGE('',*,*,#3864,.T.);
#5362=ORIENTED_EDGE('',*,*,#3865,.F.);
#5363=ORIENTED_EDGE('',*,*,#3866,.T.);
#5364=ORIENTED_EDGE('',*,*,#3867,.T.);
#5365=ORIENTED_EDGE('',*,*,#3868,.F.);
#5366=ORIENTED_EDGE('',*,*,#3869,.T.);
#5367=ORIENTED_EDGE('',*,*,#3870,.T.);
#5368=ORIENTED_EDGE('',*,*,#3871,.F.);
#5369=ORIENTED_EDGE('',*,*,#3872,.T.);
#5370=ORIENTED_EDGE('',*,*,#3873,.T.);
#5371=ORIENTED_EDGE('',*,*,#3874,.F.);
#5372=ORIENTED_EDGE('',*,*,#3875,.T.);
#5373=ORIENTED_EDGE('',*,*,#3876,.T.);
#5374=ORIENTED_EDGE('',*,*,#3877,.F.);
#5375=ORIENTED_EDGE('',*,*,#3878,.T.);
#5376=ORIENTED_EDGE('',*,*,#3879,.T.);
#5377=ORIENTED_EDGE('',*,*,#3880,.F.);
#5378=ORIENTED_EDGE('',*,*,#3881,.T.);
#5379=ORIENTED_EDGE('',*,*,#3882,.T.);
#5380=ORIENTED_EDGE('',*,*,#3883,.F.);
#5381=ORIENTED_EDGE('',*,*,#3884,.T.);
#5382=ORIENTED_EDGE('',*,*,#3885,.T.);
#5383=ORIENTED_EDGE('',*,*,#3886,.F.);
#5384=ORIENTED_EDGE('',*,*,#3887,.T.);
#5385=ORIENTED_EDGE('',*,*,#3888,.T.);
#5386=ORIENTED_EDGE('',*,*,#3889,.F.);
#5387=ORIENTED_EDGE('',*,*,#3890,.T.);
#5388=ORIENTED_EDGE('',*,*,#3891,.T.);
#5389=ORIENTED_EDGE('',*,*,#3892,.F.);
#5390=ORIENTED_EDGE('',*,*,#3893,.T.);
#5391=ORIENTED_EDGE('',*,*,#3894,.T.);
#5392=ORIENTED_EDGE('',*,*,#3895,.F.);
#5393=ORIENTED_EDGE('',*,*,#3896,.T.);
#5394=ORIENTED_EDGE('',*,*,#3897,.T.);
#5395=ORIENTED_EDGE('',*,*,#3898,.F.);
#5396=ORIENTED_EDGE('',*,*,#3899,.T.);
#5397=ORIENTED_EDGE('',*,*,#3900,.T.);
#5398=ORIENTED_EDGE('',*,*,#3901,.F.);
#5399=ORIENTED_EDGE('',*,*,#3902,.T.);
#5400=ORIENTED_EDGE('',*,*,#3903,.T.);
#5401=ORIENTED_EDGE('',*,*,#3904,.F.);
#5402=ORIENTED_EDGE('',*,*,#3905,.T.);
#5403=ORIENTED_EDGE('',*,*,#3906,.T.);
#5404=ORIENTED_EDGE('',*,*,#3907,.F.);
#5405=ORIENTED_EDGE('',*,*,#3908,.T.);
#5406=ORIENTED_EDGE('',*,*,#3909,.T.);
#5407=ORIENTED_EDGE('',*,*,#3910,.F.);
#5408=ORIENTED_EDGE('',*,*,#3911,.T.);
#5409=ORIENTED_EDGE('',*,*,#3912,.T.);
#5410=ORIENTED_EDGE('',*,*,#3913,.F.);
#5411=ORIENTED_EDGE('',*,*,#3914,.T.);
#5412=ORIENTED_EDGE('',*,*,#3915,.T.);
#5413=ORIENTED_EDGE('',*,*,#3848,.F.);
#5414=ORIENTED_EDGE('',*,*,#3852,.T.);
#5415=ORIENTED_EDGE('',*,*,#3853,.T.);
#5416=ORIENTED_EDGE('',*,*,#3916,.T.);
#5417=ORIENTED_EDGE('',*,*,#3917,.T.);
#5418=ORIENTED_EDGE('',*,*,#3916,.F.);
#5419=ORIENTED_EDGE('',*,*,#3918,.F.);
#5420=ORIENTED_EDGE('',*,*,#3917,.F.);
#5421=ORIENTED_EDGE('',*,*,#3918,.T.);
#5422=ORIENTED_EDGE('',*,*,#3919,.T.);
#5423=ORIENTED_EDGE('',*,*,#3920,.T.);
#5424=ORIENTED_EDGE('',*,*,#3921,.T.);
#5425=ORIENTED_EDGE('',*,*,#3919,.F.);
#5426=ORIENTED_EDGE('',*,*,#3920,.F.);
#5427=ORIENTED_EDGE('',*,*,#3921,.F.);
#5428=ORIENTED_EDGE('',*,*,#3922,.T.);
#5429=ORIENTED_EDGE('',*,*,#3833,.T.);
#5430=ORIENTED_EDGE('',*,*,#3923,.T.);
#5431=ORIENTED_EDGE('',*,*,#3924,.T.);
#5432=ORIENTED_EDGE('',*,*,#3923,.F.);
#5433=ORIENTED_EDGE('',*,*,#3832,.T.);
#5434=ORIENTED_EDGE('',*,*,#3834,.T.);
#5435=ORIENTED_EDGE('',*,*,#3922,.F.);
#5436=ORIENTED_EDGE('',*,*,#3841,.T.);
#5437=ORIENTED_EDGE('',*,*,#3844,.T.);
#5438=ORIENTED_EDGE('',*,*,#3925,.F.);
#5439=ORIENTED_EDGE('',*,*,#3926,.F.);
#5440=ORIENTED_EDGE('',*,*,#3927,.F.);
#5441=ORIENTED_EDGE('',*,*,#3928,.F.);
#5442=ORIENTED_EDGE('',*,*,#3929,.F.);
#5443=ORIENTED_EDGE('',*,*,#3930,.F.);
#5444=ORIENTED_EDGE('',*,*,#3931,.F.);
#5445=ORIENTED_EDGE('',*,*,#3932,.F.);
#5446=ORIENTED_EDGE('',*,*,#3933,.F.);
#5447=ORIENTED_EDGE('',*,*,#3934,.F.);
#5448=ORIENTED_EDGE('',*,*,#3935,.F.);
#5449=ORIENTED_EDGE('',*,*,#3936,.F.);
#5450=ORIENTED_EDGE('',*,*,#3937,.F.);
#5451=ORIENTED_EDGE('',*,*,#3938,.F.);
#5452=ORIENTED_EDGE('',*,*,#3939,.F.);
#5453=ORIENTED_EDGE('',*,*,#3940,.F.);
#5454=ORIENTED_EDGE('',*,*,#3941,.F.);
#5455=ORIENTED_EDGE('',*,*,#3942,.F.);
#5456=ORIENTED_EDGE('',*,*,#3943,.F.);
#5457=ORIENTED_EDGE('',*,*,#3944,.F.);
#5458=ORIENTED_EDGE('',*,*,#3945,.F.);
#5459=ORIENTED_EDGE('',*,*,#3946,.F.);
#5460=ORIENTED_EDGE('',*,*,#3947,.F.);
#5461=ORIENTED_EDGE('',*,*,#3948,.F.);
#5462=ORIENTED_EDGE('',*,*,#3949,.F.);
#5463=ORIENTED_EDGE('',*,*,#3950,.F.);
#5464=ORIENTED_EDGE('',*,*,#3951,.F.);
#5465=ORIENTED_EDGE('',*,*,#3952,.F.);
#5466=ORIENTED_EDGE('',*,*,#3953,.F.);
#5467=ORIENTED_EDGE('',*,*,#3954,.F.);
#5468=ORIENTED_EDGE('',*,*,#3955,.F.);
#5469=ORIENTED_EDGE('',*,*,#3956,.F.);
#5470=ORIENTED_EDGE('',*,*,#3957,.F.);
#5471=ORIENTED_EDGE('',*,*,#3958,.F.);
#5472=ORIENTED_EDGE('',*,*,#3959,.F.);
#5473=ORIENTED_EDGE('',*,*,#3960,.F.);
#5474=ORIENTED_EDGE('',*,*,#3961,.F.);
#5475=ORIENTED_EDGE('',*,*,#3962,.F.);
#5476=ORIENTED_EDGE('',*,*,#3963,.F.);
#5477=ORIENTED_EDGE('',*,*,#3964,.F.);
#5478=ORIENTED_EDGE('',*,*,#3965,.F.);
#5479=ORIENTED_EDGE('',*,*,#3966,.F.);
#5480=ORIENTED_EDGE('',*,*,#3967,.F.);
#5481=ORIENTED_EDGE('',*,*,#3968,.F.);
#5482=ORIENTED_EDGE('',*,*,#3969,.F.);
#5483=ORIENTED_EDGE('',*,*,#3970,.F.);
#5484=ORIENTED_EDGE('',*,*,#3971,.F.);
#5485=ORIENTED_EDGE('',*,*,#3972,.F.);
#5486=ORIENTED_EDGE('',*,*,#3973,.F.);
#5487=ORIENTED_EDGE('',*,*,#3974,.F.);
#5488=ORIENTED_EDGE('',*,*,#3975,.F.);
#5489=ORIENTED_EDGE('',*,*,#3976,.F.);
#5490=ORIENTED_EDGE('',*,*,#3977,.F.);
#5491=ORIENTED_EDGE('',*,*,#3978,.F.);
#5492=ORIENTED_EDGE('',*,*,#3979,.F.);
#5493=ORIENTED_EDGE('',*,*,#3980,.F.);
#5494=ORIENTED_EDGE('',*,*,#3981,.F.);
#5495=ORIENTED_EDGE('',*,*,#3982,.F.);
#5496=ORIENTED_EDGE('',*,*,#3983,.T.);
#5497=ORIENTED_EDGE('',*,*,#3984,.F.);
#5498=ORIENTED_EDGE('',*,*,#3983,.F.);
#5499=ORIENTED_EDGE('',*,*,#3984,.T.);
#5500=ORIENTED_EDGE('',*,*,#3985,.T.);
#5501=ORIENTED_EDGE('',*,*,#3986,.F.);
#5502=ORIENTED_EDGE('',*,*,#3985,.F.);
#5503=ORIENTED_EDGE('',*,*,#3987,.F.);
#5504=ORIENTED_EDGE('',*,*,#3988,.F.);
#5505=ORIENTED_EDGE('',*,*,#3989,.F.);
#5506=ORIENTED_EDGE('',*,*,#3988,.T.);
#5507=ORIENTED_EDGE('',*,*,#3990,.F.);
#5508=ORIENTED_EDGE('',*,*,#3914,.F.);
#5509=ORIENTED_EDGE('',*,*,#3991,.F.);
#5510=ORIENTED_EDGE('',*,*,#3992,.T.);
#5511=ORIENTED_EDGE('',*,*,#3980,.T.);
#5512=ORIENTED_EDGE('',*,*,#3993,.F.);
#5513=ORIENTED_EDGE('',*,*,#3857,.F.);
#5514=ORIENTED_EDGE('',*,*,#3994,.F.);
#5515=ORIENTED_EDGE('',*,*,#3995,.T.);
#5516=ORIENTED_EDGE('',*,*,#3977,.T.);
#5517=ORIENTED_EDGE('',*,*,#3996,.F.);
#5518=ORIENTED_EDGE('',*,*,#3860,.F.);
#5519=ORIENTED_EDGE('',*,*,#3997,.F.);
#5520=ORIENTED_EDGE('',*,*,#3998,.T.);
#5521=ORIENTED_EDGE('',*,*,#3974,.T.);
#5522=ORIENTED_EDGE('',*,*,#3999,.F.);
#5523=ORIENTED_EDGE('',*,*,#3863,.F.);
#5524=ORIENTED_EDGE('',*,*,#4000,.F.);
#5525=ORIENTED_EDGE('',*,*,#4001,.T.);
#5526=ORIENTED_EDGE('',*,*,#3971,.T.);
#5527=ORIENTED_EDGE('',*,*,#4002,.F.);
#5528=ORIENTED_EDGE('',*,*,#3866,.F.);
#5529=ORIENTED_EDGE('',*,*,#4003,.F.);
#5530=ORIENTED_EDGE('',*,*,#4004,.T.);
#5531=ORIENTED_EDGE('',*,*,#3968,.T.);
#5532=ORIENTED_EDGE('',*,*,#4005,.F.);
#5533=ORIENTED_EDGE('',*,*,#3869,.F.);
#5534=ORIENTED_EDGE('',*,*,#4006,.F.);
#5535=ORIENTED_EDGE('',*,*,#4007,.T.);
#5536=ORIENTED_EDGE('',*,*,#3965,.T.);
#5537=ORIENTED_EDGE('',*,*,#4008,.F.);
#5538=ORIENTED_EDGE('',*,*,#3872,.F.);
#5539=ORIENTED_EDGE('',*,*,#4009,.F.);
#5540=ORIENTED_EDGE('',*,*,#4010,.T.);
#5541=ORIENTED_EDGE('',*,*,#3962,.T.);
#5542=ORIENTED_EDGE('',*,*,#4011,.F.);
#5543=ORIENTED_EDGE('',*,*,#3875,.F.);
#5544=ORIENTED_EDGE('',*,*,#4012,.F.);
#5545=ORIENTED_EDGE('',*,*,#4013,.T.);
#5546=ORIENTED_EDGE('',*,*,#3959,.T.);
#5547=ORIENTED_EDGE('',*,*,#4014,.F.);
#5548=ORIENTED_EDGE('',*,*,#3878,.F.);
#5549=ORIENTED_EDGE('',*,*,#4015,.F.);
#5550=ORIENTED_EDGE('',*,*,#4016,.T.);
#5551=ORIENTED_EDGE('',*,*,#3956,.T.);
#5552=ORIENTED_EDGE('',*,*,#4017,.F.);
#5553=ORIENTED_EDGE('',*,*,#3881,.F.);
#5554=ORIENTED_EDGE('',*,*,#4018,.F.);
#5555=ORIENTED_EDGE('',*,*,#4019,.T.);
#5556=ORIENTED_EDGE('',*,*,#3953,.T.);
#5557=ORIENTED_EDGE('',*,*,#4020,.F.);
#5558=ORIENTED_EDGE('',*,*,#3884,.F.);
#5559=ORIENTED_EDGE('',*,*,#4021,.F.);
#5560=ORIENTED_EDGE('',*,*,#4022,.T.);
#5561=ORIENTED_EDGE('',*,*,#3950,.T.);
#5562=ORIENTED_EDGE('',*,*,#4023,.F.);
#5563=ORIENTED_EDGE('',*,*,#3887,.F.);
#5564=ORIENTED_EDGE('',*,*,#4024,.F.);
#5565=ORIENTED_EDGE('',*,*,#4025,.T.);
#5566=ORIENTED_EDGE('',*,*,#3947,.T.);
#5567=ORIENTED_EDGE('',*,*,#4026,.F.);
#5568=ORIENTED_EDGE('',*,*,#3890,.F.);
#5569=ORIENTED_EDGE('',*,*,#4027,.F.);
#5570=ORIENTED_EDGE('',*,*,#4028,.T.);
#5571=ORIENTED_EDGE('',*,*,#3944,.T.);
#5572=ORIENTED_EDGE('',*,*,#4029,.F.);
#5573=ORIENTED_EDGE('',*,*,#3893,.F.);
#5574=ORIENTED_EDGE('',*,*,#4030,.F.);
#5575=ORIENTED_EDGE('',*,*,#4031,.T.);
#5576=ORIENTED_EDGE('',*,*,#3941,.T.);
#5577=ORIENTED_EDGE('',*,*,#4032,.F.);
#5578=ORIENTED_EDGE('',*,*,#3896,.F.);
#5579=ORIENTED_EDGE('',*,*,#4033,.F.);
#5580=ORIENTED_EDGE('',*,*,#4034,.T.);
#5581=ORIENTED_EDGE('',*,*,#3938,.T.);
#5582=ORIENTED_EDGE('',*,*,#4035,.F.);
#5583=ORIENTED_EDGE('',*,*,#3899,.F.);
#5584=ORIENTED_EDGE('',*,*,#4036,.F.);
#5585=ORIENTED_EDGE('',*,*,#4037,.T.);
#5586=ORIENTED_EDGE('',*,*,#3935,.T.);
#5587=ORIENTED_EDGE('',*,*,#4038,.F.);
#5588=ORIENTED_EDGE('',*,*,#3902,.F.);
#5589=ORIENTED_EDGE('',*,*,#4039,.F.);
#5590=ORIENTED_EDGE('',*,*,#4040,.T.);
#5591=ORIENTED_EDGE('',*,*,#3932,.T.);
#5592=ORIENTED_EDGE('',*,*,#4041,.F.);
#5593=ORIENTED_EDGE('',*,*,#3905,.F.);
#5594=ORIENTED_EDGE('',*,*,#4042,.F.);
#5595=ORIENTED_EDGE('',*,*,#4043,.T.);
#5596=ORIENTED_EDGE('',*,*,#3929,.T.);
#5597=ORIENTED_EDGE('',*,*,#4044,.F.);
#5598=ORIENTED_EDGE('',*,*,#3908,.F.);
#5599=ORIENTED_EDGE('',*,*,#4045,.F.);
#5600=ORIENTED_EDGE('',*,*,#4046,.T.);
#5601=ORIENTED_EDGE('',*,*,#3926,.T.);
#5602=ORIENTED_EDGE('',*,*,#4047,.F.);
#5603=ORIENTED_EDGE('',*,*,#3911,.F.);
#5604=ORIENTED_EDGE('',*,*,#4048,.F.);
#5605=ORIENTED_EDGE('',*,*,#4049,.T.);
#5606=ORIENTED_EDGE('',*,*,#3987,.T.);
#5607=ORIENTED_EDGE('',*,*,#4050,.T.);
#5608=ORIENTED_EDGE('',*,*,#4051,.F.);
#5609=ORIENTED_EDGE('',*,*,#3915,.F.);
#5610=ORIENTED_EDGE('',*,*,#3990,.T.);
#5611=ORIENTED_EDGE('',*,*,#3989,.T.);
#5612=ORIENTED_EDGE('',*,*,#3992,.F.);
#5613=ORIENTED_EDGE('',*,*,#4052,.F.);
#5614=ORIENTED_EDGE('',*,*,#4050,.F.);
#5615=ORIENTED_EDGE('',*,*,#3982,.T.);
#5616=ORIENTED_EDGE('',*,*,#4053,.T.);
#5617=ORIENTED_EDGE('',*,*,#4054,.T.);
#5618=ORIENTED_EDGE('',*,*,#4018,.T.);
#5619=ORIENTED_EDGE('',*,*,#3880,.T.);
#5620=ORIENTED_EDGE('',*,*,#4055,.T.);
#5621=ORIENTED_EDGE('',*,*,#4056,.T.);
#5622=ORIENTED_EDGE('',*,*,#4015,.T.);
#5623=ORIENTED_EDGE('',*,*,#3877,.T.);
#5624=ORIENTED_EDGE('',*,*,#4057,.T.);
#5625=ORIENTED_EDGE('',*,*,#4058,.T.);
#5626=ORIENTED_EDGE('',*,*,#4012,.T.);
#5627=ORIENTED_EDGE('',*,*,#3874,.T.);
#5628=ORIENTED_EDGE('',*,*,#4059,.T.);
#5629=ORIENTED_EDGE('',*,*,#4060,.T.);
#5630=ORIENTED_EDGE('',*,*,#4009,.T.);
#5631=ORIENTED_EDGE('',*,*,#3871,.T.);
#5632=ORIENTED_EDGE('',*,*,#4061,.T.);
#5633=ORIENTED_EDGE('',*,*,#4062,.T.);
#5634=ORIENTED_EDGE('',*,*,#4006,.T.);
#5635=ORIENTED_EDGE('',*,*,#3868,.T.);
#5636=ORIENTED_EDGE('',*,*,#4063,.T.);
#5637=ORIENTED_EDGE('',*,*,#4064,.T.);
#5638=ORIENTED_EDGE('',*,*,#4003,.T.);
#5639=ORIENTED_EDGE('',*,*,#3865,.T.);
#5640=ORIENTED_EDGE('',*,*,#4065,.T.);
#5641=ORIENTED_EDGE('',*,*,#4066,.T.);
#5642=ORIENTED_EDGE('',*,*,#4000,.T.);
#5643=ORIENTED_EDGE('',*,*,#3862,.T.);
#5644=ORIENTED_EDGE('',*,*,#4067,.T.);
#5645=ORIENTED_EDGE('',*,*,#4068,.T.);
#5646=ORIENTED_EDGE('',*,*,#3997,.T.);
#5647=ORIENTED_EDGE('',*,*,#3859,.T.);
#5648=ORIENTED_EDGE('',*,*,#4069,.T.);
#5649=ORIENTED_EDGE('',*,*,#4070,.T.);
#5650=ORIENTED_EDGE('',*,*,#3994,.T.);
#5651=ORIENTED_EDGE('',*,*,#3856,.T.);
#5652=ORIENTED_EDGE('',*,*,#4051,.T.);
#5653=ORIENTED_EDGE('',*,*,#4052,.T.);
#5654=ORIENTED_EDGE('',*,*,#3991,.T.);
#5655=ORIENTED_EDGE('',*,*,#3913,.T.);
#5656=ORIENTED_EDGE('',*,*,#4071,.T.);
#5657=ORIENTED_EDGE('',*,*,#4072,.T.);
#5658=ORIENTED_EDGE('',*,*,#4048,.T.);
#5659=ORIENTED_EDGE('',*,*,#3910,.T.);
#5660=ORIENTED_EDGE('',*,*,#4073,.T.);
#5661=ORIENTED_EDGE('',*,*,#4074,.T.);
#5662=ORIENTED_EDGE('',*,*,#4045,.T.);
#5663=ORIENTED_EDGE('',*,*,#3907,.T.);
#5664=ORIENTED_EDGE('',*,*,#4075,.T.);
#5665=ORIENTED_EDGE('',*,*,#4076,.T.);
#5666=ORIENTED_EDGE('',*,*,#4042,.T.);
#5667=ORIENTED_EDGE('',*,*,#3904,.T.);
#5668=ORIENTED_EDGE('',*,*,#4077,.T.);
#5669=ORIENTED_EDGE('',*,*,#4078,.T.);
#5670=ORIENTED_EDGE('',*,*,#4039,.T.);
#5671=ORIENTED_EDGE('',*,*,#3901,.T.);
#5672=ORIENTED_EDGE('',*,*,#4079,.T.);
#5673=ORIENTED_EDGE('',*,*,#4080,.T.);
#5674=ORIENTED_EDGE('',*,*,#4036,.T.);
#5675=ORIENTED_EDGE('',*,*,#3898,.T.);
#5676=ORIENTED_EDGE('',*,*,#4081,.T.);
#5677=ORIENTED_EDGE('',*,*,#4082,.T.);
#5678=ORIENTED_EDGE('',*,*,#4033,.T.);
#5679=ORIENTED_EDGE('',*,*,#3895,.T.);
#5680=ORIENTED_EDGE('',*,*,#4083,.T.);
#5681=ORIENTED_EDGE('',*,*,#4084,.T.);
#5682=ORIENTED_EDGE('',*,*,#4030,.T.);
#5683=ORIENTED_EDGE('',*,*,#3892,.T.);
#5684=ORIENTED_EDGE('',*,*,#4085,.T.);
#5685=ORIENTED_EDGE('',*,*,#4086,.T.);
#5686=ORIENTED_EDGE('',*,*,#4027,.T.);
#5687=ORIENTED_EDGE('',*,*,#3889,.T.);
#5688=ORIENTED_EDGE('',*,*,#4087,.T.);
#5689=ORIENTED_EDGE('',*,*,#4088,.T.);
#5690=ORIENTED_EDGE('',*,*,#4024,.T.);
#5691=ORIENTED_EDGE('',*,*,#3886,.T.);
#5692=ORIENTED_EDGE('',*,*,#4089,.T.);
#5693=ORIENTED_EDGE('',*,*,#4090,.T.);
#5694=ORIENTED_EDGE('',*,*,#4021,.T.);
#5695=ORIENTED_EDGE('',*,*,#3883,.T.);
#5696=ORIENTED_EDGE('',*,*,#4091,.T.);
#5697=ORIENTED_EDGE('',*,*,#4092,.T.);
#5698=ORIENTED_EDGE('',*,*,#4053,.F.);
#5699=ORIENTED_EDGE('',*,*,#3979,.T.);
#5700=ORIENTED_EDGE('',*,*,#4093,.T.);
#5701=ORIENTED_EDGE('',*,*,#4069,.F.);
#5702=ORIENTED_EDGE('',*,*,#3858,.F.);
#5703=ORIENTED_EDGE('',*,*,#3993,.T.);
#5704=ORIENTED_EDGE('',*,*,#3981,.T.);
#5705=ORIENTED_EDGE('',*,*,#3995,.F.);
#5706=ORIENTED_EDGE('',*,*,#4070,.F.);
#5707=ORIENTED_EDGE('',*,*,#4093,.F.);
#5708=ORIENTED_EDGE('',*,*,#3976,.T.);
#5709=ORIENTED_EDGE('',*,*,#4094,.T.);
#5710=ORIENTED_EDGE('',*,*,#4067,.F.);
#5711=ORIENTED_EDGE('',*,*,#3861,.F.);
#5712=ORIENTED_EDGE('',*,*,#3996,.T.);
#5713=ORIENTED_EDGE('',*,*,#3978,.T.);
#5714=ORIENTED_EDGE('',*,*,#3998,.F.);
#5715=ORIENTED_EDGE('',*,*,#4068,.F.);
#5716=ORIENTED_EDGE('',*,*,#4094,.F.);
#5717=ORIENTED_EDGE('',*,*,#3973,.T.);
#5718=ORIENTED_EDGE('',*,*,#4095,.T.);
#5719=ORIENTED_EDGE('',*,*,#4065,.F.);
#5720=ORIENTED_EDGE('',*,*,#3864,.F.);
#5721=ORIENTED_EDGE('',*,*,#3999,.T.);
#5722=ORIENTED_EDGE('',*,*,#3975,.T.);
#5723=ORIENTED_EDGE('',*,*,#4001,.F.);
#5724=ORIENTED_EDGE('',*,*,#4066,.F.);
#5725=ORIENTED_EDGE('',*,*,#4095,.F.);
#5726=ORIENTED_EDGE('',*,*,#3970,.T.);
#5727=ORIENTED_EDGE('',*,*,#4096,.T.);
#5728=ORIENTED_EDGE('',*,*,#4063,.F.);
#5729=ORIENTED_EDGE('',*,*,#3867,.F.);
#5730=ORIENTED_EDGE('',*,*,#4002,.T.);
#5731=ORIENTED_EDGE('',*,*,#3972,.T.);
#5732=ORIENTED_EDGE('',*,*,#4004,.F.);
#5733=ORIENTED_EDGE('',*,*,#4064,.F.);
#5734=ORIENTED_EDGE('',*,*,#4096,.F.);
#5735=ORIENTED_EDGE('',*,*,#3967,.T.);
#5736=ORIENTED_EDGE('',*,*,#4097,.T.);
#5737=ORIENTED_EDGE('',*,*,#4061,.F.);
#5738=ORIENTED_EDGE('',*,*,#3870,.F.);
#5739=ORIENTED_EDGE('',*,*,#4005,.T.);
#5740=ORIENTED_EDGE('',*,*,#3969,.T.);
#5741=ORIENTED_EDGE('',*,*,#4007,.F.);
#5742=ORIENTED_EDGE('',*,*,#4062,.F.);
#5743=ORIENTED_EDGE('',*,*,#4097,.F.);
#5744=ORIENTED_EDGE('',*,*,#3964,.T.);
#5745=ORIENTED_EDGE('',*,*,#4098,.T.);
#5746=ORIENTED_EDGE('',*,*,#4059,.F.);
#5747=ORIENTED_EDGE('',*,*,#3873,.F.);
#5748=ORIENTED_EDGE('',*,*,#4008,.T.);
#5749=ORIENTED_EDGE('',*,*,#3966,.T.);
#5750=ORIENTED_EDGE('',*,*,#4010,.F.);
#5751=ORIENTED_EDGE('',*,*,#4060,.F.);
#5752=ORIENTED_EDGE('',*,*,#4098,.F.);
#5753=ORIENTED_EDGE('',*,*,#3961,.T.);
#5754=ORIENTED_EDGE('',*,*,#4099,.T.);
#5755=ORIENTED_EDGE('',*,*,#4057,.F.);
#5756=ORIENTED_EDGE('',*,*,#3876,.F.);
#5757=ORIENTED_EDGE('',*,*,#4011,.T.);
#5758=ORIENTED_EDGE('',*,*,#3963,.T.);
#5759=ORIENTED_EDGE('',*,*,#4013,.F.);
#5760=ORIENTED_EDGE('',*,*,#4058,.F.);
#5761=ORIENTED_EDGE('',*,*,#4099,.F.);
#5762=ORIENTED_EDGE('',*,*,#3958,.T.);
#5763=ORIENTED_EDGE('',*,*,#4100,.T.);
#5764=ORIENTED_EDGE('',*,*,#4055,.F.);
#5765=ORIENTED_EDGE('',*,*,#3879,.F.);
#5766=ORIENTED_EDGE('',*,*,#4014,.T.);
#5767=ORIENTED_EDGE('',*,*,#3960,.T.);
#5768=ORIENTED_EDGE('',*,*,#4016,.F.);
#5769=ORIENTED_EDGE('',*,*,#4056,.F.);
#5770=ORIENTED_EDGE('',*,*,#4100,.F.);
#5771=ORIENTED_EDGE('',*,*,#3955,.T.);
#5772=ORIENTED_EDGE('',*,*,#4101,.T.);
#5773=ORIENTED_EDGE('',*,*,#4091,.F.);
#5774=ORIENTED_EDGE('',*,*,#3882,.F.);
#5775=ORIENTED_EDGE('',*,*,#4017,.T.);
#5776=ORIENTED_EDGE('',*,*,#3957,.T.);
#5777=ORIENTED_EDGE('',*,*,#4019,.F.);
#5778=ORIENTED_EDGE('',*,*,#4054,.F.);
#5779=ORIENTED_EDGE('',*,*,#4092,.F.);
#5780=ORIENTED_EDGE('',*,*,#4101,.F.);
#5781=ORIENTED_EDGE('',*,*,#3952,.T.);
#5782=ORIENTED_EDGE('',*,*,#4102,.T.);
#5783=ORIENTED_EDGE('',*,*,#4089,.F.);
#5784=ORIENTED_EDGE('',*,*,#3885,.F.);
#5785=ORIENTED_EDGE('',*,*,#4020,.T.);
#5786=ORIENTED_EDGE('',*,*,#3954,.T.);
#5787=ORIENTED_EDGE('',*,*,#4022,.F.);
#5788=ORIENTED_EDGE('',*,*,#4090,.F.);
#5789=ORIENTED_EDGE('',*,*,#4102,.F.);
#5790=ORIENTED_EDGE('',*,*,#3949,.T.);
#5791=ORIENTED_EDGE('',*,*,#4103,.T.);
#5792=ORIENTED_EDGE('',*,*,#4087,.F.);
#5793=ORIENTED_EDGE('',*,*,#3888,.F.);
#5794=ORIENTED_EDGE('',*,*,#4023,.T.);
#5795=ORIENTED_EDGE('',*,*,#3951,.T.);
#5796=ORIENTED_EDGE('',*,*,#4025,.F.);
#5797=ORIENTED_EDGE('',*,*,#4088,.F.);
#5798=ORIENTED_EDGE('',*,*,#4103,.F.);
#5799=ORIENTED_EDGE('',*,*,#3946,.T.);
#5800=ORIENTED_EDGE('',*,*,#4104,.T.);
#5801=ORIENTED_EDGE('',*,*,#4085,.F.);
#5802=ORIENTED_EDGE('',*,*,#3891,.F.);
#5803=ORIENTED_EDGE('',*,*,#4026,.T.);
#5804=ORIENTED_EDGE('',*,*,#3948,.T.);
#5805=ORIENTED_EDGE('',*,*,#4028,.F.);
#5806=ORIENTED_EDGE('',*,*,#4086,.F.);
#5807=ORIENTED_EDGE('',*,*,#4104,.F.);
#5808=ORIENTED_EDGE('',*,*,#3943,.T.);
#5809=ORIENTED_EDGE('',*,*,#4105,.T.);
#5810=ORIENTED_EDGE('',*,*,#4083,.F.);
#5811=ORIENTED_EDGE('',*,*,#3894,.F.);
#5812=ORIENTED_EDGE('',*,*,#4029,.T.);
#5813=ORIENTED_EDGE('',*,*,#3945,.T.);
#5814=ORIENTED_EDGE('',*,*,#4031,.F.);
#5815=ORIENTED_EDGE('',*,*,#4084,.F.);
#5816=ORIENTED_EDGE('',*,*,#4105,.F.);
#5817=ORIENTED_EDGE('',*,*,#3940,.T.);
#5818=ORIENTED_EDGE('',*,*,#4106,.T.);
#5819=ORIENTED_EDGE('',*,*,#4081,.F.);
#5820=ORIENTED_EDGE('',*,*,#3897,.F.);
#5821=ORIENTED_EDGE('',*,*,#4032,.T.);
#5822=ORIENTED_EDGE('',*,*,#3942,.T.);
#5823=ORIENTED_EDGE('',*,*,#4034,.F.);
#5824=ORIENTED_EDGE('',*,*,#4082,.F.);
#5825=ORIENTED_EDGE('',*,*,#4106,.F.);
#5826=ORIENTED_EDGE('',*,*,#3937,.T.);
#5827=ORIENTED_EDGE('',*,*,#4107,.T.);
#5828=ORIENTED_EDGE('',*,*,#4079,.F.);
#5829=ORIENTED_EDGE('',*,*,#3900,.F.);
#5830=ORIENTED_EDGE('',*,*,#4035,.T.);
#5831=ORIENTED_EDGE('',*,*,#3939,.T.);
#5832=ORIENTED_EDGE('',*,*,#4037,.F.);
#5833=ORIENTED_EDGE('',*,*,#4080,.F.);
#5834=ORIENTED_EDGE('',*,*,#4107,.F.);
#5835=ORIENTED_EDGE('',*,*,#3934,.T.);
#5836=ORIENTED_EDGE('',*,*,#4108,.T.);
#5837=ORIENTED_EDGE('',*,*,#4077,.F.);
#5838=ORIENTED_EDGE('',*,*,#3903,.F.);
#5839=ORIENTED_EDGE('',*,*,#4038,.T.);
#5840=ORIENTED_EDGE('',*,*,#3936,.T.);
#5841=ORIENTED_EDGE('',*,*,#4040,.F.);
#5842=ORIENTED_EDGE('',*,*,#4078,.F.);
#5843=ORIENTED_EDGE('',*,*,#4108,.F.);
#5844=ORIENTED_EDGE('',*,*,#3931,.T.);
#5845=ORIENTED_EDGE('',*,*,#4109,.T.);
#5846=ORIENTED_EDGE('',*,*,#4075,.F.);
#5847=ORIENTED_EDGE('',*,*,#3906,.F.);
#5848=ORIENTED_EDGE('',*,*,#4041,.T.);
#5849=ORIENTED_EDGE('',*,*,#3933,.T.);
#5850=ORIENTED_EDGE('',*,*,#4043,.F.);
#5851=ORIENTED_EDGE('',*,*,#4076,.F.);
#5852=ORIENTED_EDGE('',*,*,#4109,.F.);
#5853=ORIENTED_EDGE('',*,*,#3928,.T.);
#5854=ORIENTED_EDGE('',*,*,#4110,.T.);
#5855=ORIENTED_EDGE('',*,*,#4073,.F.);
#5856=ORIENTED_EDGE('',*,*,#3909,.F.);
#5857=ORIENTED_EDGE('',*,*,#4044,.T.);
#5858=ORIENTED_EDGE('',*,*,#3930,.T.);
#5859=ORIENTED_EDGE('',*,*,#4046,.F.);
#5860=ORIENTED_EDGE('',*,*,#4074,.F.);
#5861=ORIENTED_EDGE('',*,*,#4110,.F.);
#5862=ORIENTED_EDGE('',*,*,#3925,.T.);
#5863=ORIENTED_EDGE('',*,*,#4111,.T.);
#5864=ORIENTED_EDGE('',*,*,#4071,.F.);
#5865=ORIENTED_EDGE('',*,*,#3912,.F.);
#5866=ORIENTED_EDGE('',*,*,#4047,.T.);
#5867=ORIENTED_EDGE('',*,*,#3927,.T.);
#5868=ORIENTED_EDGE('',*,*,#4049,.F.);
#5869=ORIENTED_EDGE('',*,*,#4072,.F.);
#5870=ORIENTED_EDGE('',*,*,#4111,.F.);
#5871=ORIENTED_EDGE('',*,*,#3986,.T.);
#5872=ORIENTED_EDGE('',*,*,#3924,.F.);
#5873=ORIENTED_EDGE('',*,*,#4112,.F.);
#5874=ORIENTED_EDGE('',*,*,#4113,.T.);
#5875=ORIENTED_EDGE('',*,*,#4114,.F.);
#5876=ORIENTED_EDGE('',*,*,#4115,.F.);
#5877=ORIENTED_EDGE('',*,*,#4116,.T.);
#5878=ORIENTED_EDGE('',*,*,#4117,.F.);
#5879=ORIENTED_EDGE('',*,*,#4118,.F.);
#5880=ORIENTED_EDGE('',*,*,#4116,.F.);
#5881=ORIENTED_EDGE('',*,*,#4119,.F.);
#5882=ORIENTED_EDGE('',*,*,#4113,.F.);
#5883=ORIENTED_EDGE('',*,*,#4120,.F.);
#5884=ORIENTED_EDGE('',*,*,#4121,.T.);
#5885=ORIENTED_EDGE('',*,*,#4122,.F.);
#5886=ORIENTED_EDGE('',*,*,#4123,.F.);
#5887=ORIENTED_EDGE('',*,*,#4124,.F.);
#5888=ORIENTED_EDGE('',*,*,#4121,.F.);
#5889=ORIENTED_EDGE('',*,*,#4125,.F.);
#5890=ORIENTED_EDGE('',*,*,#4123,.T.);
#5891=ORIENTED_EDGE('',*,*,#4126,.T.);
#5892=ORIENTED_EDGE('',*,*,#4127,.T.);
#5893=ORIENTED_EDGE('',*,*,#4126,.F.);
#5894=ORIENTED_EDGE('',*,*,#4127,.F.);
#5895=ORIENTED_EDGE('',*,*,#4128,.T.);
#5896=ORIENTED_EDGE('',*,*,#4129,.F.);
#5897=ORIENTED_EDGE('',*,*,#4128,.F.);
#5898=ORIENTED_EDGE('',*,*,#4130,.F.);
#5899=ORIENTED_EDGE('',*,*,#4131,.T.);
#5900=ORIENTED_EDGE('',*,*,#4132,.T.);
#5901=ORIENTED_EDGE('',*,*,#4131,.F.);
#5902=ORIENTED_EDGE('',*,*,#4132,.F.);
#5903=ORIENTED_EDGE('',*,*,#4133,.T.);
#5904=ORIENTED_EDGE('',*,*,#4133,.F.);
#5905=ORIENTED_EDGE('',*,*,#4134,.F.);
#5906=ORIENTED_EDGE('',*,*,#4130,.T.);
#5907=ORIENTED_EDGE('',*,*,#4135,.F.);
#5908=ORIENTED_EDGE('',*,*,#4136,.T.);
#5909=ORIENTED_EDGE('',*,*,#4134,.T.);
#5910=ORIENTED_EDGE('',*,*,#4136,.F.);
#5911=ORIENTED_EDGE('',*,*,#4137,.F.);
#5912=ORIENTED_EDGE('',*,*,#4138,.T.);
#5913=ORIENTED_EDGE('',*,*,#4117,.T.);
#5914=ORIENTED_EDGE('',*,*,#4118,.T.);
#5915=ORIENTED_EDGE('',*,*,#4112,.T.);
#5916=ORIENTED_EDGE('',*,*,#4139,.T.);
#5917=ORIENTED_EDGE('',*,*,#4135,.T.);
#5918=ORIENTED_EDGE('',*,*,#4139,.F.);
#5919=ORIENTED_EDGE('',*,*,#4114,.T.);
#5920=ORIENTED_EDGE('',*,*,#4119,.T.);
#5921=ORIENTED_EDGE('',*,*,#4115,.T.);
#5922=ORIENTED_EDGE('',*,*,#4138,.F.);
#5923=ORIENTED_EDGE('',*,*,#4124,.T.);
#5924=ORIENTED_EDGE('',*,*,#4125,.T.);
#5925=ORIENTED_EDGE('',*,*,#4122,.T.);
#5926=ORIENTED_EDGE('',*,*,#4120,.T.);
#5927=ORIENTED_EDGE('',*,*,#4140,.F.);
#5928=ORIENTED_EDGE('',*,*,#4141,.T.);
#5929=ORIENTED_EDGE('',*,*,#4137,.T.);
#5930=ORIENTED_EDGE('',*,*,#4141,.F.);
#5931=ORIENTED_EDGE('',*,*,#4140,.T.);
#5932=ORIENTED_EDGE('',*,*,#4129,.T.);
#5933=ORIENTED_EDGE('',*,*,#4142,.F.);
#5934=ORIENTED_EDGE('',*,*,#4143,.T.);
#5935=ORIENTED_EDGE('',*,*,#4144,.F.);
#5936=ORIENTED_EDGE('',*,*,#4145,.F.);
#5937=ORIENTED_EDGE('',*,*,#4146,.T.);
#5938=ORIENTED_EDGE('',*,*,#4147,.F.);
#5939=ORIENTED_EDGE('',*,*,#4148,.F.);
#5940=ORIENTED_EDGE('',*,*,#4146,.F.);
#5941=ORIENTED_EDGE('',*,*,#4149,.F.);
#5942=ORIENTED_EDGE('',*,*,#4143,.F.);
#5943=ORIENTED_EDGE('',*,*,#4150,.F.);
#5944=ORIENTED_EDGE('',*,*,#4151,.T.);
#5945=ORIENTED_EDGE('',*,*,#4152,.F.);
#5946=ORIENTED_EDGE('',*,*,#4153,.F.);
#5947=ORIENTED_EDGE('',*,*,#4154,.F.);
#5948=ORIENTED_EDGE('',*,*,#4151,.F.);
#5949=ORIENTED_EDGE('',*,*,#4155,.F.);
#5950=ORIENTED_EDGE('',*,*,#4153,.T.);
#5951=ORIENTED_EDGE('',*,*,#4156,.T.);
#5952=ORIENTED_EDGE('',*,*,#4157,.T.);
#5953=ORIENTED_EDGE('',*,*,#4156,.F.);
#5954=ORIENTED_EDGE('',*,*,#4157,.F.);
#5955=ORIENTED_EDGE('',*,*,#4158,.T.);
#5956=ORIENTED_EDGE('',*,*,#4159,.F.);
#5957=ORIENTED_EDGE('',*,*,#4158,.F.);
#5958=ORIENTED_EDGE('',*,*,#4160,.F.);
#5959=ORIENTED_EDGE('',*,*,#4161,.T.);
#5960=ORIENTED_EDGE('',*,*,#4162,.T.);
#5961=ORIENTED_EDGE('',*,*,#4161,.F.);
#5962=ORIENTED_EDGE('',*,*,#4162,.F.);
#5963=ORIENTED_EDGE('',*,*,#4163,.T.);
#5964=ORIENTED_EDGE('',*,*,#4163,.F.);
#5965=ORIENTED_EDGE('',*,*,#4164,.F.);
#5966=ORIENTED_EDGE('',*,*,#4160,.T.);
#5967=ORIENTED_EDGE('',*,*,#4165,.F.);
#5968=ORIENTED_EDGE('',*,*,#4166,.T.);
#5969=ORIENTED_EDGE('',*,*,#4164,.T.);
#5970=ORIENTED_EDGE('',*,*,#4166,.F.);
#5971=ORIENTED_EDGE('',*,*,#4167,.F.);
#5972=ORIENTED_EDGE('',*,*,#4168,.T.);
#5973=ORIENTED_EDGE('',*,*,#4147,.T.);
#5974=ORIENTED_EDGE('',*,*,#4148,.T.);
#5975=ORIENTED_EDGE('',*,*,#4142,.T.);
#5976=ORIENTED_EDGE('',*,*,#4169,.T.);
#5977=ORIENTED_EDGE('',*,*,#4165,.T.);
#5978=ORIENTED_EDGE('',*,*,#4169,.F.);
#5979=ORIENTED_EDGE('',*,*,#4144,.T.);
#5980=ORIENTED_EDGE('',*,*,#4149,.T.);
#5981=ORIENTED_EDGE('',*,*,#4145,.T.);
#5982=ORIENTED_EDGE('',*,*,#4168,.F.);
#5983=ORIENTED_EDGE('',*,*,#4154,.T.);
#5984=ORIENTED_EDGE('',*,*,#4155,.T.);
#5985=ORIENTED_EDGE('',*,*,#4152,.T.);
#5986=ORIENTED_EDGE('',*,*,#4150,.T.);
#5987=ORIENTED_EDGE('',*,*,#4170,.F.);
#5988=ORIENTED_EDGE('',*,*,#4171,.T.);
#5989=ORIENTED_EDGE('',*,*,#4167,.T.);
#5990=ORIENTED_EDGE('',*,*,#4171,.F.);
#5991=ORIENTED_EDGE('',*,*,#4170,.T.);
#5992=ORIENTED_EDGE('',*,*,#4159,.T.);
#5993=ORIENTED_EDGE('',*,*,#4172,.T.);
#5994=ORIENTED_EDGE('',*,*,#4172,.F.);
#5995=ORIENTED_EDGE('',*,*,#4173,.F.);
#5996=ORIENTED_EDGE('',*,*,#4174,.F.);
#5997=ORIENTED_EDGE('',*,*,#4175,.F.);
#5998=ORIENTED_EDGE('',*,*,#4176,.F.);
#5999=ORIENTED_EDGE('',*,*,#4177,.F.);
#6000=ORIENTED_EDGE('',*,*,#4178,.F.);
#6001=ORIENTED_EDGE('',*,*,#4179,.F.);
#6002=ORIENTED_EDGE('',*,*,#4180,.F.);
#6003=ORIENTED_EDGE('',*,*,#4181,.T.);
#6004=ORIENTED_EDGE('',*,*,#4182,.T.);
#6005=ORIENTED_EDGE('',*,*,#4183,.T.);
#6006=ORIENTED_EDGE('',*,*,#4184,.F.);
#6007=ORIENTED_EDGE('',*,*,#4185,.T.);
#6008=ORIENTED_EDGE('',*,*,#4186,.F.);
#6009=ORIENTED_EDGE('',*,*,#4187,.T.);
#6010=ORIENTED_EDGE('',*,*,#4188,.F.);
#6011=ORIENTED_EDGE('',*,*,#4189,.T.);
#6012=ORIENTED_EDGE('',*,*,#4190,.F.);
#6013=ORIENTED_EDGE('',*,*,#4191,.T.);
#6014=ORIENTED_EDGE('',*,*,#4192,.F.);
#6015=ORIENTED_EDGE('',*,*,#4193,.T.);
#6016=ORIENTED_EDGE('',*,*,#4194,.F.);
#6017=ORIENTED_EDGE('',*,*,#4175,.T.);
#6018=ORIENTED_EDGE('',*,*,#4195,.F.);
#6019=ORIENTED_EDGE('',*,*,#4196,.T.);
#6020=ORIENTED_EDGE('',*,*,#4197,.F.);
#6021=ORIENTED_EDGE('',*,*,#4198,.T.);
#6022=ORIENTED_EDGE('',*,*,#4199,.F.);
#6023=ORIENTED_EDGE('',*,*,#4200,.T.);
#6024=ORIENTED_EDGE('',*,*,#4201,.F.);
#6025=ORIENTED_EDGE('',*,*,#4202,.T.);
#6026=ORIENTED_EDGE('',*,*,#4182,.F.);
#6027=ORIENTED_EDGE('',*,*,#4174,.T.);
#6028=ORIENTED_EDGE('',*,*,#4203,.F.);
#6029=ORIENTED_EDGE('',*,*,#4204,.T.);
#6030=ORIENTED_EDGE('',*,*,#4195,.T.);
#6031=ORIENTED_EDGE('',*,*,#4179,.T.);
#6032=ORIENTED_EDGE('',*,*,#4205,.F.);
#6033=ORIENTED_EDGE('',*,*,#4206,.T.);
#6034=ORIENTED_EDGE('',*,*,#4207,.F.);
#6035=ORIENTED_EDGE('',*,*,#4208,.T.);
#6036=ORIENTED_EDGE('',*,*,#4209,.F.);
#6037=ORIENTED_EDGE('',*,*,#4210,.T.);
#6038=ORIENTED_EDGE('',*,*,#4211,.F.);
#6039=ORIENTED_EDGE('',*,*,#4212,.T.);
#6040=ORIENTED_EDGE('',*,*,#4213,.T.);
#6041=ORIENTED_EDGE('',*,*,#4214,.T.);
#6042=ORIENTED_EDGE('',*,*,#4213,.F.);
#6043=ORIENTED_EDGE('',*,*,#4215,.T.);
#6044=ORIENTED_EDGE('',*,*,#4216,.F.);
#6045=ORIENTED_EDGE('',*,*,#4217,.T.);
#6046=ORIENTED_EDGE('',*,*,#4218,.F.);
#6047=ORIENTED_EDGE('',*,*,#4219,.T.);
#6048=ORIENTED_EDGE('',*,*,#4220,.F.);
#6049=ORIENTED_EDGE('',*,*,#4221,.T.);
#6050=ORIENTED_EDGE('',*,*,#4222,.F.);
#6051=ORIENTED_EDGE('',*,*,#4223,.T.);
#6052=ORIENTED_EDGE('',*,*,#4224,.F.);
#6053=ORIENTED_EDGE('',*,*,#4225,.T.);
#6054=ORIENTED_EDGE('',*,*,#4226,.F.);
#6055=ORIENTED_EDGE('',*,*,#4178,.T.);
#6056=ORIENTED_EDGE('',*,*,#4227,.F.);
#6057=ORIENTED_EDGE('',*,*,#4228,.T.);
#6058=ORIENTED_EDGE('',*,*,#4205,.T.);
#6059=ORIENTED_EDGE('',*,*,#4229,.T.);
#6060=ORIENTED_EDGE('',*,*,#4229,.F.);
#6061=ORIENTED_EDGE('',*,*,#4230,.F.);
#6062=ORIENTED_EDGE('',*,*,#4231,.F.);
#6063=ORIENTED_EDGE('',*,*,#4196,.F.);
#6064=ORIENTED_EDGE('',*,*,#4204,.F.);
#6065=ORIENTED_EDGE('',*,*,#4232,.F.);
#6066=ORIENTED_EDGE('',*,*,#4233,.F.);
#6067=ORIENTED_EDGE('',*,*,#4206,.F.);
#6068=ORIENTED_EDGE('',*,*,#4228,.F.);
#6069=ORIENTED_EDGE('',*,*,#4231,.T.);
#6070=ORIENTED_EDGE('',*,*,#4234,.F.);
#6071=ORIENTED_EDGE('',*,*,#4235,.T.);
#6072=ORIENTED_EDGE('',*,*,#4197,.T.);
#6073=ORIENTED_EDGE('',*,*,#4233,.T.);
#6074=ORIENTED_EDGE('',*,*,#4236,.F.);
#6075=ORIENTED_EDGE('',*,*,#4237,.T.);
#6076=ORIENTED_EDGE('',*,*,#4207,.T.);
#6077=ORIENTED_EDGE('',*,*,#4238,.T.);
#6078=ORIENTED_EDGE('',*,*,#4238,.F.);
#6079=ORIENTED_EDGE('',*,*,#4239,.F.);
#6080=ORIENTED_EDGE('',*,*,#4240,.F.);
#6081=ORIENTED_EDGE('',*,*,#4198,.F.);
#6082=ORIENTED_EDGE('',*,*,#4235,.F.);
#6083=ORIENTED_EDGE('',*,*,#4241,.F.);
#6084=ORIENTED_EDGE('',*,*,#4242,.F.);
#6085=ORIENTED_EDGE('',*,*,#4208,.F.);
#6086=ORIENTED_EDGE('',*,*,#4237,.F.);
#6087=ORIENTED_EDGE('',*,*,#4240,.T.);
#6088=ORIENTED_EDGE('',*,*,#4243,.F.);
#6089=ORIENTED_EDGE('',*,*,#4244,.T.);
#6090=ORIENTED_EDGE('',*,*,#4199,.T.);
#6091=ORIENTED_EDGE('',*,*,#4242,.T.);
#6092=ORIENTED_EDGE('',*,*,#4245,.F.);
#6093=ORIENTED_EDGE('',*,*,#4246,.T.);
#6094=ORIENTED_EDGE('',*,*,#4209,.T.);
#6095=ORIENTED_EDGE('',*,*,#4247,.T.);
#6096=ORIENTED_EDGE('',*,*,#4247,.F.);
#6097=ORIENTED_EDGE('',*,*,#4248,.F.);
#6098=ORIENTED_EDGE('',*,*,#4249,.F.);
#6099=ORIENTED_EDGE('',*,*,#4200,.F.);
#6100=ORIENTED_EDGE('',*,*,#4244,.F.);
#6101=ORIENTED_EDGE('',*,*,#4250,.F.);
#6102=ORIENTED_EDGE('',*,*,#4251,.F.);
#6103=ORIENTED_EDGE('',*,*,#4210,.F.);
#6104=ORIENTED_EDGE('',*,*,#4246,.F.);
#6105=ORIENTED_EDGE('',*,*,#4249,.T.);
#6106=ORIENTED_EDGE('',*,*,#4252,.F.);
#6107=ORIENTED_EDGE('',*,*,#4253,.T.);
#6108=ORIENTED_EDGE('',*,*,#4201,.T.);
#6109=ORIENTED_EDGE('',*,*,#4251,.T.);
#6110=ORIENTED_EDGE('',*,*,#4254,.F.);
#6111=ORIENTED_EDGE('',*,*,#4255,.T.);
#6112=ORIENTED_EDGE('',*,*,#4211,.T.);
#6113=ORIENTED_EDGE('',*,*,#4256,.T.);
#6114=ORIENTED_EDGE('',*,*,#4256,.F.);
#6115=ORIENTED_EDGE('',*,*,#4257,.F.);
#6116=ORIENTED_EDGE('',*,*,#4258,.F.);
#6117=ORIENTED_EDGE('',*,*,#4183,.F.);
#6118=ORIENTED_EDGE('',*,*,#4202,.F.);
#6119=ORIENTED_EDGE('',*,*,#4253,.F.);
#6120=ORIENTED_EDGE('',*,*,#4259,.F.);
#6121=ORIENTED_EDGE('',*,*,#4260,.F.);
#6122=ORIENTED_EDGE('',*,*,#4261,.F.);
#6123=ORIENTED_EDGE('',*,*,#4215,.F.);
#6124=ORIENTED_EDGE('',*,*,#4212,.F.);
#6125=ORIENTED_EDGE('',*,*,#4255,.F.);
#6126=ORIENTED_EDGE('',*,*,#4262,.F.);
#6127=ORIENTED_EDGE('',*,*,#4258,.T.);
#6128=ORIENTED_EDGE('',*,*,#4263,.F.);
#6129=ORIENTED_EDGE('',*,*,#4264,.T.);
#6130=ORIENTED_EDGE('',*,*,#4184,.T.);
#6131=ORIENTED_EDGE('',*,*,#4261,.T.);
#6132=ORIENTED_EDGE('',*,*,#4265,.F.);
#6133=ORIENTED_EDGE('',*,*,#4266,.T.);
#6134=ORIENTED_EDGE('',*,*,#4216,.T.);
#6135=ORIENTED_EDGE('',*,*,#4267,.T.);
#6136=ORIENTED_EDGE('',*,*,#4267,.F.);
#6137=ORIENTED_EDGE('',*,*,#4268,.F.);
#6138=ORIENTED_EDGE('',*,*,#4269,.F.);
#6139=ORIENTED_EDGE('',*,*,#4185,.F.);
#6140=ORIENTED_EDGE('',*,*,#4264,.F.);
#6141=ORIENTED_EDGE('',*,*,#4270,.F.);
#6142=ORIENTED_EDGE('',*,*,#4271,.F.);
#6143=ORIENTED_EDGE('',*,*,#4217,.F.);
#6144=ORIENTED_EDGE('',*,*,#4266,.F.);
#6145=ORIENTED_EDGE('',*,*,#4269,.T.);
#6146=ORIENTED_EDGE('',*,*,#4272,.F.);
#6147=ORIENTED_EDGE('',*,*,#4273,.T.);
#6148=ORIENTED_EDGE('',*,*,#4186,.T.);
#6149=ORIENTED_EDGE('',*,*,#4271,.T.);
#6150=ORIENTED_EDGE('',*,*,#4274,.F.);
#6151=ORIENTED_EDGE('',*,*,#4275,.T.);
#6152=ORIENTED_EDGE('',*,*,#4218,.T.);
#6153=ORIENTED_EDGE('',*,*,#4276,.T.);
#6154=ORIENTED_EDGE('',*,*,#4276,.F.);
#6155=ORIENTED_EDGE('',*,*,#4277,.F.);
#6156=ORIENTED_EDGE('',*,*,#4278,.F.);
#6157=ORIENTED_EDGE('',*,*,#4187,.F.);
#6158=ORIENTED_EDGE('',*,*,#4273,.F.);
#6159=ORIENTED_EDGE('',*,*,#4279,.F.);
#6160=ORIENTED_EDGE('',*,*,#4280,.F.);
#6161=ORIENTED_EDGE('',*,*,#4219,.F.);
#6162=ORIENTED_EDGE('',*,*,#4275,.F.);
#6163=ORIENTED_EDGE('',*,*,#4278,.T.);
#6164=ORIENTED_EDGE('',*,*,#4281,.F.);
#6165=ORIENTED_EDGE('',*,*,#4282,.T.);
#6166=ORIENTED_EDGE('',*,*,#4188,.T.);
#6167=ORIENTED_EDGE('',*,*,#4280,.T.);
#6168=ORIENTED_EDGE('',*,*,#4283,.F.);
#6169=ORIENTED_EDGE('',*,*,#4284,.T.);
#6170=ORIENTED_EDGE('',*,*,#4220,.T.);
#6171=ORIENTED_EDGE('',*,*,#4285,.T.);
#6172=ORIENTED_EDGE('',*,*,#4285,.F.);
#6173=ORIENTED_EDGE('',*,*,#4286,.F.);
#6174=ORIENTED_EDGE('',*,*,#4287,.F.);
#6175=ORIENTED_EDGE('',*,*,#4189,.F.);
#6176=ORIENTED_EDGE('',*,*,#4282,.F.);
#6177=ORIENTED_EDGE('',*,*,#4288,.F.);
#6178=ORIENTED_EDGE('',*,*,#4289,.F.);
#6179=ORIENTED_EDGE('',*,*,#4221,.F.);
#6180=ORIENTED_EDGE('',*,*,#4284,.F.);
#6181=ORIENTED_EDGE('',*,*,#4287,.T.);
#6182=ORIENTED_EDGE('',*,*,#4290,.F.);
#6183=ORIENTED_EDGE('',*,*,#4291,.T.);
#6184=ORIENTED_EDGE('',*,*,#4190,.T.);
#6185=ORIENTED_EDGE('',*,*,#4289,.T.);
#6186=ORIENTED_EDGE('',*,*,#4292,.F.);
#6187=ORIENTED_EDGE('',*,*,#4293,.T.);
#6188=ORIENTED_EDGE('',*,*,#4222,.T.);
#6189=ORIENTED_EDGE('',*,*,#4294,.T.);
#6190=ORIENTED_EDGE('',*,*,#4294,.F.);
#6191=ORIENTED_EDGE('',*,*,#4191,.F.);
#6192=ORIENTED_EDGE('',*,*,#4291,.F.);
#6193=ORIENTED_EDGE('',*,*,#4295,.F.);
#6194=ORIENTED_EDGE('',*,*,#4296,.F.);
#6195=ORIENTED_EDGE('',*,*,#4223,.F.);
#6196=ORIENTED_EDGE('',*,*,#4293,.F.);
#6197=ORIENTED_EDGE('',*,*,#4297,.F.);
#6198=ORIENTED_EDGE('',*,*,#4298,.F.);
#6199=ORIENTED_EDGE('',*,*,#4173,.T.);
#6200=ORIENTED_EDGE('',*,*,#4299,.T.);
#6201=ORIENTED_EDGE('',*,*,#4300,.T.);
#6202=ORIENTED_EDGE('',*,*,#4301,.T.);
#6203=ORIENTED_EDGE('',*,*,#4295,.T.);
#6204=ORIENTED_EDGE('',*,*,#4290,.T.);
#6205=ORIENTED_EDGE('',*,*,#4286,.T.);
#6206=ORIENTED_EDGE('',*,*,#4281,.T.);
#6207=ORIENTED_EDGE('',*,*,#4277,.T.);
#6208=ORIENTED_EDGE('',*,*,#4272,.T.);
#6209=ORIENTED_EDGE('',*,*,#4268,.T.);
#6210=ORIENTED_EDGE('',*,*,#4263,.T.);
#6211=ORIENTED_EDGE('',*,*,#4257,.T.);
#6212=ORIENTED_EDGE('',*,*,#4302,.T.);
#6213=ORIENTED_EDGE('',*,*,#4303,.F.);
#6214=ORIENTED_EDGE('',*,*,#4302,.F.);
#6215=ORIENTED_EDGE('',*,*,#4259,.T.);
#6216=ORIENTED_EDGE('',*,*,#4252,.T.);
#6217=ORIENTED_EDGE('',*,*,#4248,.T.);
#6218=ORIENTED_EDGE('',*,*,#4243,.T.);
#6219=ORIENTED_EDGE('',*,*,#4239,.T.);
#6220=ORIENTED_EDGE('',*,*,#4234,.T.);
#6221=ORIENTED_EDGE('',*,*,#4230,.T.);
#6222=ORIENTED_EDGE('',*,*,#4203,.T.);
#6223=ORIENTED_EDGE('',*,*,#4176,.T.);
#6224=ORIENTED_EDGE('',*,*,#4194,.T.);
#6225=ORIENTED_EDGE('',*,*,#4304,.T.);
#6226=ORIENTED_EDGE('',*,*,#4299,.F.);
#6227=ORIENTED_EDGE('',*,*,#4305,.F.);
#6228=ORIENTED_EDGE('',*,*,#4306,.T.);
#6229=ORIENTED_EDGE('',*,*,#4262,.T.);
#6230=ORIENTED_EDGE('',*,*,#4254,.T.);
#6231=ORIENTED_EDGE('',*,*,#4250,.T.);
#6232=ORIENTED_EDGE('',*,*,#4245,.T.);
#6233=ORIENTED_EDGE('',*,*,#4241,.T.);
#6234=ORIENTED_EDGE('',*,*,#4236,.T.);
#6235=ORIENTED_EDGE('',*,*,#4232,.T.);
#6236=ORIENTED_EDGE('',*,*,#4227,.T.);
#6237=ORIENTED_EDGE('',*,*,#4177,.T.);
#6238=ORIENTED_EDGE('',*,*,#4307,.T.);
#6239=ORIENTED_EDGE('',*,*,#4308,.T.);
#6240=ORIENTED_EDGE('',*,*,#4309,.T.);
#6241=ORIENTED_EDGE('',*,*,#4297,.T.);
#6242=ORIENTED_EDGE('',*,*,#4292,.T.);
#6243=ORIENTED_EDGE('',*,*,#4288,.T.);
#6244=ORIENTED_EDGE('',*,*,#4283,.T.);
#6245=ORIENTED_EDGE('',*,*,#4279,.T.);
#6246=ORIENTED_EDGE('',*,*,#4274,.T.);
#6247=ORIENTED_EDGE('',*,*,#4270,.T.);
#6248=ORIENTED_EDGE('',*,*,#4265,.T.);
#6249=ORIENTED_EDGE('',*,*,#4260,.T.);
#6250=ORIENTED_EDGE('',*,*,#4306,.F.);
#6251=ORIENTED_EDGE('',*,*,#4180,.T.);
#6252=ORIENTED_EDGE('',*,*,#4226,.T.);
#6253=ORIENTED_EDGE('',*,*,#4310,.T.);
#6254=ORIENTED_EDGE('',*,*,#4307,.F.);
#6255=ORIENTED_EDGE('',*,*,#4311,.T.);
#6256=ORIENTED_EDGE('',*,*,#4311,.F.);
#6257=ORIENTED_EDGE('',*,*,#4310,.F.);
#6258=ORIENTED_EDGE('',*,*,#4225,.F.);
#6259=ORIENTED_EDGE('',*,*,#4312,.F.);
#6260=ORIENTED_EDGE('',*,*,#4308,.F.);
#6261=ORIENTED_EDGE('',*,*,#4304,.F.);
#6262=ORIENTED_EDGE('',*,*,#4193,.F.);
#6263=ORIENTED_EDGE('',*,*,#4313,.F.);
#6264=ORIENTED_EDGE('',*,*,#4300,.F.);
#6265=ORIENTED_EDGE('',*,*,#4296,.T.);
#6266=ORIENTED_EDGE('',*,*,#4301,.F.);
#6267=ORIENTED_EDGE('',*,*,#4313,.T.);
#6268=ORIENTED_EDGE('',*,*,#4192,.T.);
#6269=ORIENTED_EDGE('',*,*,#4314,.F.);
#6270=ORIENTED_EDGE('',*,*,#4303,.T.);
#6271=ORIENTED_EDGE('',*,*,#4315,.F.);
#6272=ORIENTED_EDGE('',*,*,#4316,.T.);
#6273=ORIENTED_EDGE('',*,*,#4314,.T.);
#6274=ORIENTED_EDGE('',*,*,#4316,.F.);
#6275=ORIENTED_EDGE('',*,*,#4317,.F.);
#6276=ORIENTED_EDGE('',*,*,#4318,.T.);
#6277=ORIENTED_EDGE('',*,*,#4315,.T.);
#6278=ORIENTED_EDGE('',*,*,#4318,.F.);
#6279=ORIENTED_EDGE('',*,*,#4319,.F.);
#6280=ORIENTED_EDGE('',*,*,#4320,.T.);
#6281=ORIENTED_EDGE('',*,*,#4317,.T.);
#6282=ORIENTED_EDGE('',*,*,#4320,.F.);
#6283=ORIENTED_EDGE('',*,*,#4319,.T.);
#6284=ORIENTED_EDGE('',*,*,#4321,.F.);
#6285=ORIENTED_EDGE('',*,*,#4321,.T.);
#6286=ORIENTED_EDGE('',*,*,#4322,.T.);
#6287=ORIENTED_EDGE('',*,*,#4181,.F.);
#6288=ORIENTED_EDGE('',*,*,#4322,.F.);
#6289=ORIENTED_EDGE('',*,*,#4298,.T.);
#6290=ORIENTED_EDGE('',*,*,#4309,.F.);
#6291=ORIENTED_EDGE('',*,*,#4312,.T.);
#6292=ORIENTED_EDGE('',*,*,#4224,.T.);
#6293=ORIENTED_EDGE('',*,*,#4305,.T.);
#6294=ORIENTED_EDGE('',*,*,#4323,.F.);
#6295=ORIENTED_EDGE('',*,*,#4323,.T.);
#6296=ORIENTED_EDGE('',*,*,#4324,.T.);
#6297=ORIENTED_EDGE('',*,*,#4325,.F.);
#6298=ORIENTED_EDGE('',*,*,#4324,.F.);
#6299=ORIENTED_EDGE('',*,*,#4325,.T.);
#6300=ORIENTED_EDGE('',*,*,#4326,.T.);
#6301=ORIENTED_EDGE('',*,*,#4327,.F.);
#6302=ORIENTED_EDGE('',*,*,#4326,.F.);
#6303=ORIENTED_EDGE('',*,*,#4327,.T.);
#6304=ORIENTED_EDGE('',*,*,#4328,.T.);
#6305=ORIENTED_EDGE('',*,*,#4329,.F.);
#6306=ORIENTED_EDGE('',*,*,#4328,.F.);
#6307=ORIENTED_EDGE('',*,*,#4214,.F.);
#6308=ORIENTED_EDGE('',*,*,#4329,.T.);
#6309=ORIENTED_EDGE('',*,*,#4330,.F.);
#6310=ORIENTED_EDGE('',*,*,#4331,.T.);
#6311=ORIENTED_EDGE('',*,*,#4332,.F.);
#6312=ORIENTED_EDGE('',*,*,#4333,.T.);
#6313=ORIENTED_EDGE('',*,*,#4330,.T.);
#6314=ORIENTED_EDGE('',*,*,#4333,.F.);
#6315=ORIENTED_EDGE('',*,*,#4334,.F.);
#6316=ORIENTED_EDGE('',*,*,#4332,.T.);
#6317=ORIENTED_EDGE('',*,*,#4334,.T.);
#6318=ORIENTED_EDGE('',*,*,#4335,.T.);
#6319=ORIENTED_EDGE('',*,*,#4336,.F.);
#6320=ORIENTED_EDGE('',*,*,#4335,.F.);
#6321=ORIENTED_EDGE('',*,*,#4337,.F.);
#6322=ORIENTED_EDGE('',*,*,#4336,.T.);
#6323=ORIENTED_EDGE('',*,*,#4338,.F.);
#6324=ORIENTED_EDGE('',*,*,#4339,.T.);
#6325=ORIENTED_EDGE('',*,*,#4337,.T.);
#6326=ORIENTED_EDGE('',*,*,#4339,.F.);
#6327=ORIENTED_EDGE('',*,*,#4340,.F.);
#6328=ORIENTED_EDGE('',*,*,#4341,.T.);
#6329=ORIENTED_EDGE('',*,*,#4338,.T.);
#6330=ORIENTED_EDGE('',*,*,#4341,.F.);
#6331=ORIENTED_EDGE('',*,*,#4342,.F.);
#6332=ORIENTED_EDGE('',*,*,#4343,.T.);
#6333=ORIENTED_EDGE('',*,*,#4340,.T.);
#6334=ORIENTED_EDGE('',*,*,#4343,.F.);
#6335=ORIENTED_EDGE('',*,*,#4342,.T.);
#6336=ORIENTED_EDGE('',*,*,#4344,.F.);
#6337=ORIENTED_EDGE('',*,*,#4344,.T.);
#6338=ORIENTED_EDGE('',*,*,#4345,.T.);
#6339=ORIENTED_EDGE('',*,*,#4346,.F.);
#6340=ORIENTED_EDGE('',*,*,#4345,.F.);
#6341=ORIENTED_EDGE('',*,*,#4346,.T.);
#6342=ORIENTED_EDGE('',*,*,#4347,.F.);
#6343=ORIENTED_EDGE('',*,*,#4348,.F.);
#6344=ORIENTED_EDGE('',*,*,#4349,.T.);
#6345=ORIENTED_EDGE('',*,*,#4347,.T.);
#6346=ORIENTED_EDGE('',*,*,#4349,.F.);
#6347=ORIENTED_EDGE('',*,*,#4348,.T.);
#6348=ORIENTED_EDGE('',*,*,#4350,.F.);
#6349=ORIENTED_EDGE('',*,*,#4350,.T.);
#6350=ORIENTED_EDGE('',*,*,#4351,.T.);
#6351=ORIENTED_EDGE('',*,*,#4352,.F.);
#6352=ORIENTED_EDGE('',*,*,#4351,.F.);
#6353=ORIENTED_EDGE('',*,*,#4352,.T.);
#6354=ORIENTED_EDGE('',*,*,#4353,.T.);
#6355=ORIENTED_EDGE('',*,*,#4354,.F.);
#6356=ORIENTED_EDGE('',*,*,#4353,.F.);
#6357=ORIENTED_EDGE('',*,*,#4354,.T.);
#6358=ORIENTED_EDGE('',*,*,#4355,.T.);
#6359=ORIENTED_EDGE('',*,*,#4331,.F.);
#6360=ORIENTED_EDGE('',*,*,#4355,.F.);
#6361=ORIENTED_EDGE('',*,*,#4356,.F.);
#6362=ORIENTED_EDGE('',*,*,#4357,.T.);
#6363=ORIENTED_EDGE('',*,*,#4358,.T.);
#6364=ORIENTED_EDGE('',*,*,#4357,.F.);
#6365=ORIENTED_EDGE('',*,*,#4356,.T.);
#6366=ORIENTED_EDGE('',*,*,#4359,.F.);
#6367=ORIENTED_EDGE('',*,*,#4359,.T.);
#6368=ORIENTED_EDGE('',*,*,#4360,.T.);
#6369=ORIENTED_EDGE('',*,*,#4361,.F.);
#6370=ORIENTED_EDGE('',*,*,#4360,.F.);
#6371=ORIENTED_EDGE('',*,*,#4358,.F.);
#6372=ORIENTED_EDGE('',*,*,#4361,.T.);
#6373=ORIENTED_EDGE('',*,*,#4362,.F.);
#6374=ORIENTED_EDGE('',*,*,#4363,.T.);
#6375=ORIENTED_EDGE('',*,*,#4364,.T.);
#6376=ORIENTED_EDGE('',*,*,#4365,.T.);
#6377=ORIENTED_EDGE('',*,*,#4366,.F.);
#6378=ORIENTED_EDGE('',*,*,#4367,.T.);
#6379=ORIENTED_EDGE('',*,*,#4362,.T.);
#6380=ORIENTED_EDGE('',*,*,#4368,.T.);
#6381=ORIENTED_EDGE('',*,*,#4369,.F.);
#6382=ORIENTED_EDGE('',*,*,#4370,.T.);
#6383=ORIENTED_EDGE('',*,*,#4366,.T.);
#6384=ORIENTED_EDGE('',*,*,#4371,.T.);
#6385=ORIENTED_EDGE('',*,*,#4372,.F.);
#6386=ORIENTED_EDGE('',*,*,#4373,.T.);
#6387=ORIENTED_EDGE('',*,*,#4369,.T.);
#6388=ORIENTED_EDGE('',*,*,#4374,.T.);
#6389=ORIENTED_EDGE('',*,*,#4375,.F.);
#6390=ORIENTED_EDGE('',*,*,#4376,.T.);
#6391=ORIENTED_EDGE('',*,*,#4372,.T.);
#6392=ORIENTED_EDGE('',*,*,#4377,.T.);
#6393=ORIENTED_EDGE('',*,*,#4378,.F.);
#6394=ORIENTED_EDGE('',*,*,#4379,.T.);
#6395=ORIENTED_EDGE('',*,*,#4380,.F.);
#6396=ORIENTED_EDGE('',*,*,#4381,.F.);
#6397=ORIENTED_EDGE('',*,*,#4382,.F.);
#6398=ORIENTED_EDGE('',*,*,#4383,.T.);
#6399=ORIENTED_EDGE('',*,*,#4378,.T.);
#6400=ORIENTED_EDGE('',*,*,#4384,.F.);
#6401=ORIENTED_EDGE('',*,*,#4385,.F.);
#6402=ORIENTED_EDGE('',*,*,#4386,.T.);
#6403=ORIENTED_EDGE('',*,*,#4382,.T.);
#6404=ORIENTED_EDGE('',*,*,#4387,.F.);
#6405=ORIENTED_EDGE('',*,*,#4388,.F.);
#6406=ORIENTED_EDGE('',*,*,#4389,.T.);
#6407=ORIENTED_EDGE('',*,*,#4385,.T.);
#6408=ORIENTED_EDGE('',*,*,#4390,.F.);
#6409=ORIENTED_EDGE('',*,*,#4380,.T.);
#6410=ORIENTED_EDGE('',*,*,#4391,.T.);
#6411=ORIENTED_EDGE('',*,*,#4392,.F.);
#6412=ORIENTED_EDGE('',*,*,#4393,.F.);
#6413=ORIENTED_EDGE('',*,*,#4394,.T.);
#6414=ORIENTED_EDGE('',*,*,#4394,.F.);
#6415=ORIENTED_EDGE('',*,*,#4395,.F.);
#6416=ORIENTED_EDGE('',*,*,#4377,.F.);
#6417=ORIENTED_EDGE('',*,*,#4374,.F.);
#6418=ORIENTED_EDGE('',*,*,#4371,.F.);
#6419=ORIENTED_EDGE('',*,*,#4368,.F.);
#6420=ORIENTED_EDGE('',*,*,#4365,.F.);
#6421=ORIENTED_EDGE('',*,*,#4396,.F.);
#6422=ORIENTED_EDGE('',*,*,#4397,.T.);
#6423=ORIENTED_EDGE('',*,*,#4390,.T.);
#6424=ORIENTED_EDGE('',*,*,#4387,.T.);
#6425=ORIENTED_EDGE('',*,*,#4384,.T.);
#6426=ORIENTED_EDGE('',*,*,#4381,.T.);
#6427=ORIENTED_EDGE('',*,*,#4398,.T.);
#6428=ORIENTED_EDGE('',*,*,#4399,.T.);
#6429=ORIENTED_EDGE('',*,*,#4400,.T.);
#6430=ORIENTED_EDGE('',*,*,#4401,.T.);
#6431=ORIENTED_EDGE('',*,*,#4396,.T.);
#6432=ORIENTED_EDGE('',*,*,#4388,.T.);
#6433=ORIENTED_EDGE('',*,*,#4397,.F.);
#6434=ORIENTED_EDGE('',*,*,#4401,.F.);
#6435=ORIENTED_EDGE('',*,*,#4402,.T.);
#6436=ORIENTED_EDGE('',*,*,#4391,.F.);
#6437=ORIENTED_EDGE('',*,*,#4379,.F.);
#6438=ORIENTED_EDGE('',*,*,#4383,.F.);
#6439=ORIENTED_EDGE('',*,*,#4386,.F.);
#6440=ORIENTED_EDGE('',*,*,#4389,.F.);
#6441=ORIENTED_EDGE('',*,*,#4402,.F.);
#6442=ORIENTED_EDGE('',*,*,#4400,.F.);
#6443=ORIENTED_EDGE('',*,*,#4363,.F.);
#6444=ORIENTED_EDGE('',*,*,#4367,.F.);
#6445=ORIENTED_EDGE('',*,*,#4370,.F.);
#6446=ORIENTED_EDGE('',*,*,#4373,.F.);
#6447=ORIENTED_EDGE('',*,*,#4376,.F.);
#6448=ORIENTED_EDGE('',*,*,#4403,.F.);
#6449=ORIENTED_EDGE('',*,*,#4404,.T.);
#6450=ORIENTED_EDGE('',*,*,#4405,.F.);
#6451=ORIENTED_EDGE('',*,*,#4404,.F.);
#6452=ORIENTED_EDGE('',*,*,#4406,.F.);
#6453=ORIENTED_EDGE('',*,*,#4407,.F.);
#6454=ORIENTED_EDGE('',*,*,#4408,.F.);
#6455=ORIENTED_EDGE('',*,*,#4409,.T.);
#6456=ORIENTED_EDGE('',*,*,#4410,.F.);
#6457=ORIENTED_EDGE('',*,*,#4409,.F.);
#6458=ORIENTED_EDGE('',*,*,#4411,.F.);
#6459=ORIENTED_EDGE('',*,*,#4412,.T.);
#6460=ORIENTED_EDGE('',*,*,#4413,.F.);
#6461=ORIENTED_EDGE('',*,*,#4412,.F.);
#6462=ORIENTED_EDGE('',*,*,#4414,.F.);
#6463=ORIENTED_EDGE('',*,*,#4415,.T.);
#6464=ORIENTED_EDGE('',*,*,#4416,.F.);
#6465=ORIENTED_EDGE('',*,*,#4415,.F.);
#6466=ORIENTED_EDGE('',*,*,#4417,.F.);
#6467=ORIENTED_EDGE('',*,*,#4418,.T.);
#6468=ORIENTED_EDGE('',*,*,#4419,.F.);
#6469=ORIENTED_EDGE('',*,*,#4418,.F.);
#6470=ORIENTED_EDGE('',*,*,#4420,.F.);
#6471=ORIENTED_EDGE('',*,*,#4421,.T.);
#6472=ORIENTED_EDGE('',*,*,#4422,.F.);
#6473=ORIENTED_EDGE('',*,*,#4421,.F.);
#6474=ORIENTED_EDGE('',*,*,#4423,.F.);
#6475=ORIENTED_EDGE('',*,*,#4407,.T.);
#6476=ORIENTED_EDGE('',*,*,#4414,.T.);
#6477=ORIENTED_EDGE('',*,*,#4411,.T.);
#6478=ORIENTED_EDGE('',*,*,#4408,.T.);
#6479=ORIENTED_EDGE('',*,*,#4423,.T.);
#6480=ORIENTED_EDGE('',*,*,#4420,.T.);
#6481=ORIENTED_EDGE('',*,*,#4417,.T.);
#6482=ORIENTED_EDGE('',*,*,#4405,.T.);
#6483=ORIENTED_EDGE('',*,*,#4424,.F.);
#6484=ORIENTED_EDGE('',*,*,#4398,.F.);
#6485=ORIENTED_EDGE('',*,*,#4364,.F.);
#6486=ORIENTED_EDGE('',*,*,#4399,.F.);
#6487=ORIENTED_EDGE('',*,*,#4425,.T.);
#6488=ORIENTED_EDGE('',*,*,#4424,.T.);
#6489=ORIENTED_EDGE('',*,*,#4425,.F.);
#6490=ORIENTED_EDGE('',*,*,#4375,.T.);
#6491=ORIENTED_EDGE('',*,*,#4395,.T.);
#6492=ORIENTED_EDGE('',*,*,#4426,.F.);
#6493=ORIENTED_EDGE('',*,*,#4403,.T.);
#6494=ORIENTED_EDGE('',*,*,#4427,.F.);
#6495=ORIENTED_EDGE('',*,*,#4428,.T.);
#6496=ORIENTED_EDGE('',*,*,#4392,.T.);
#6497=ORIENTED_EDGE('',*,*,#4426,.T.);
#6498=ORIENTED_EDGE('',*,*,#4393,.T.);
#6499=ORIENTED_EDGE('',*,*,#4428,.F.);
#6500=ORIENTED_EDGE('',*,*,#4427,.T.);
#6501=ORIENTED_EDGE('',*,*,#4416,.T.);
#6502=ORIENTED_EDGE('',*,*,#4419,.T.);
#6503=ORIENTED_EDGE('',*,*,#4422,.T.);
#6504=ORIENTED_EDGE('',*,*,#4406,.T.);
#6505=ORIENTED_EDGE('',*,*,#4410,.T.);
#6506=ORIENTED_EDGE('',*,*,#4413,.T.);
#6507=ORIENTED_EDGE('',*,*,#4429,.F.);
#6508=ORIENTED_EDGE('',*,*,#4430,.T.);
#6509=ORIENTED_EDGE('',*,*,#4431,.F.);
#6510=ORIENTED_EDGE('',*,*,#4430,.F.);
#6511=ORIENTED_EDGE('',*,*,#4432,.F.);
#6512=ORIENTED_EDGE('',*,*,#4433,.T.);
#6513=ORIENTED_EDGE('',*,*,#4434,.F.);
#6514=ORIENTED_EDGE('',*,*,#4433,.F.);
#6515=ORIENTED_EDGE('',*,*,#4435,.T.);
#6516=ORIENTED_EDGE('',*,*,#4436,.T.);
#6517=ORIENTED_EDGE('',*,*,#4437,.T.);
#6518=ORIENTED_EDGE('',*,*,#4438,.F.);
#6519=ORIENTED_EDGE('',*,*,#4439,.F.);
#6520=ORIENTED_EDGE('',*,*,#4440,.F.);
#6521=ORIENTED_EDGE('',*,*,#4441,.F.);
#6522=ORIENTED_EDGE('',*,*,#4442,.T.);
#6523=ORIENTED_EDGE('',*,*,#4443,.T.);
#6524=ORIENTED_EDGE('',*,*,#4444,.T.);
#6525=ORIENTED_EDGE('',*,*,#4445,.T.);
#6526=ORIENTED_EDGE('',*,*,#4436,.F.);
#6527=ORIENTED_EDGE('',*,*,#4432,.T.);
#6528=ORIENTED_EDGE('',*,*,#4429,.T.);
#6529=ORIENTED_EDGE('',*,*,#4446,.F.);
#6530=ORIENTED_EDGE('',*,*,#4447,.F.);
#6531=ORIENTED_EDGE('',*,*,#4448,.F.);
#6532=ORIENTED_EDGE('',*,*,#4443,.F.);
#6533=ORIENTED_EDGE('',*,*,#4444,.F.);
#6534=ORIENTED_EDGE('',*,*,#4448,.T.);
#6535=ORIENTED_EDGE('',*,*,#4449,.F.);
#6536=ORIENTED_EDGE('',*,*,#4450,.F.);
#6537=ORIENTED_EDGE('',*,*,#4445,.F.);
#6538=ORIENTED_EDGE('',*,*,#4450,.T.);
#6539=ORIENTED_EDGE('',*,*,#4451,.F.);
#6540=ORIENTED_EDGE('',*,*,#4437,.F.);
#6541=ORIENTED_EDGE('',*,*,#4452,.F.);
#6542=ORIENTED_EDGE('',*,*,#4453,.F.);
#6543=ORIENTED_EDGE('',*,*,#4439,.T.);
#6544=ORIENTED_EDGE('',*,*,#4435,.F.);
#6545=ORIENTED_EDGE('',*,*,#4454,.F.);
#6546=ORIENTED_EDGE('',*,*,#4441,.T.);
#6547=ORIENTED_EDGE('',*,*,#4455,.T.);
#6548=ORIENTED_EDGE('',*,*,#4456,.F.);
#6549=ORIENTED_EDGE('',*,*,#4440,.T.);
#6550=ORIENTED_EDGE('',*,*,#4453,.T.);
#6551=ORIENTED_EDGE('',*,*,#4457,.F.);
#6552=ORIENTED_EDGE('',*,*,#4455,.F.);
#6553=ORIENTED_EDGE('',*,*,#4452,.T.);
#6554=ORIENTED_EDGE('',*,*,#4438,.T.);
#6555=ORIENTED_EDGE('',*,*,#4451,.T.);
#6556=ORIENTED_EDGE('',*,*,#4449,.T.);
#6557=ORIENTED_EDGE('',*,*,#4447,.T.);
#6558=ORIENTED_EDGE('',*,*,#4458,.F.);
#6559=ORIENTED_EDGE('',*,*,#4456,.T.);
#6560=ORIENTED_EDGE('',*,*,#4457,.T.);
#6561=ORIENTED_EDGE('',*,*,#4431,.T.);
#6562=ORIENTED_EDGE('',*,*,#4434,.T.);
#6563=ORIENTED_EDGE('',*,*,#4446,.T.);
#6564=ORIENTED_EDGE('',*,*,#4442,.F.);
#6565=ORIENTED_EDGE('',*,*,#4454,.T.);
#6566=ORIENTED_EDGE('',*,*,#4458,.T.);
#6567=CYLINDRICAL_SURFACE('',#7148,14.);
#6568=CYLINDRICAL_SURFACE('',#7153,14.7);
#6569=CYLINDRICAL_SURFACE('',#7157,14.);
#6570=CYLINDRICAL_SURFACE('',#7161,12.);
#6571=CYLINDRICAL_SURFACE('',#7165,14.);
#6572=CYLINDRICAL_SURFACE('',#7167,14.);
#6573=CYLINDRICAL_SURFACE('',#7172,14.7);
#6574=CYLINDRICAL_SURFACE('',#7176,14.);
#6575=CYLINDRICAL_SURFACE('',#7180,12.);
#6576=CYLINDRICAL_SURFACE('',#7182,12.);
#6577=CYLINDRICAL_SURFACE('',#7187,14.);
#6578=CYLINDRICAL_SURFACE('',#7191,14.7);
#6579=CYLINDRICAL_SURFACE('',#7195,14.);
#6580=CYLINDRICAL_SURFACE('',#7202,20.);
#6581=CYLINDRICAL_SURFACE('',#7225,2.);
#6582=CYLINDRICAL_SURFACE('',#7228,2.);
#6583=CYLINDRICAL_SURFACE('',#7263,3.);
#6584=CYLINDRICAL_SURFACE('',#7266,3.);
#6585=CYLINDRICAL_SURFACE('',#7272,3.);
#6586=CYLINDRICAL_SURFACE('',#7273,3.);
#6587=CYLINDRICAL_SURFACE('',#7275,2.);
#6588=CYLINDRICAL_SURFACE('',#7277,2.);
#6589=CYLINDRICAL_SURFACE('',#7284,2.05);
#6590=CYLINDRICAL_SURFACE('',#7287,2.05);
#6591=CYLINDRICAL_SURFACE('',#7292,6.025);
#6592=CYLINDRICAL_SURFACE('',#7322,10.);
#6593=CYLINDRICAL_SURFACE('',#7365,10.5);
#6594=CYLINDRICAL_SURFACE('',#7415,2.05);
#6595=CYLINDRICAL_SURFACE('',#7418,2.05);
#6596=CYLINDRICAL_SURFACE('',#7423,6.025);
#6597=CYLINDRICAL_SURFACE('',#7454,10.);
#6598=CYLINDRICAL_SURFACE('',#7497,10.5);
#6599=CYLINDRICAL_SURFACE('',#7559,1.25);
#6600=CYLINDRICAL_SURFACE('',#7561,1.25);
#6601=CYLINDRICAL_SURFACE('',#7569,6.);
#6602=CYLINDRICAL_SURFACE('',#7589,1.25);
#6603=CYLINDRICAL_SURFACE('',#7591,1.25);
#6604=CYLINDRICAL_SURFACE('',#7599,6.);
#6605=CYLINDRICAL_SURFACE('',#7621,8.3);
#6606=CYLINDRICAL_SURFACE('',#7679,11.7);
#6607=CYLINDRICAL_SURFACE('',#7684,8.3);
#6608=CYLINDRICAL_SURFACE('',#7696,14.);
#6609=CYLINDRICAL_SURFACE('',#7702,12.6);
#6610=CYLINDRICAL_SURFACE('',#7708,6.);
#6611=CYLINDRICAL_SURFACE('',#7727,14.);
#6612=CYLINDRICAL_SURFACE('',#7743,6.);
#6613=CYLINDRICAL_SURFACE('',#7747,9.);
#6614=CYLINDRICAL_SURFACE('',#7752,6.);
#6615=CYLINDRICAL_SURFACE('',#7756,1.954);
#6616=CYLINDRICAL_SURFACE('',#7758,1.954);
#6617=CYLINDRICAL_SURFACE('',#7759,1.954);
#6618=CYLINDRICAL_SURFACE('',#7760,1.954);
#6619=CYLINDRICAL_SURFACE('',#7761,1.954);
#6620=CYLINDRICAL_SURFACE('',#7762,1.5555);
#6621=CYLINDRICAL_SURFACE('',#7764,1.5555);
#6622=CYLINDRICAL_SURFACE('',#7765,1.5555);
#6623=CYLINDRICAL_SURFACE('',#7766,1.5555);
#6624=CYLINDRICAL_SURFACE('',#7774,1.5555);
#6625=CYLINDRICAL_SURFACE('',#7787,1.954);
#6626=CYLINDRICAL_SURFACE('',#7793,0.85);
#6627=CYLINDRICAL_SURFACE('',#7796,0.85);
#6628=CYLINDRICAL_SURFACE('',#7799,14.7);
#6629=CYLINDRICAL_SURFACE('',#7812,12.4);
#6630=ADVANCED_FACE('',(#979),#6567,.F.);
#6631=ADVANCED_FACE('',(#980,#780),#852,.F.);
#6632=ADVANCED_FACE('',(#981),#6568,.F.);
#6633=ADVANCED_FACE('',(#982,#781),#853,.F.);
#6634=ADVANCED_FACE('',(#983),#6569,.F.);
#6635=ADVANCED_FACE('',(#984,#782),#854,.F.);
#6636=ADVANCED_FACE('',(#985),#6570,.F.);
#6637=ADVANCED_FACE('',(#986,#783),#855,.F.);
#6638=ADVANCED_FACE('',(#987),#6571,.F.);
#6639=ADVANCED_FACE('',(#988),#6572,.F.);
#6640=ADVANCED_FACE('',(#989,#784),#856,.F.);
#6641=ADVANCED_FACE('',(#990),#6573,.F.);
#6642=ADVANCED_FACE('',(#991,#785),#857,.F.);
#6643=ADVANCED_FACE('',(#992),#6574,.F.);
#6644=ADVANCED_FACE('',(#993,#786),#858,.F.);
#6645=ADVANCED_FACE('',(#994),#6575,.F.);
#6646=ADVANCED_FACE('',(#995),#6576,.F.);
#6647=ADVANCED_FACE('',(#996,#787),#859,.F.);
#6648=ADVANCED_FACE('',(#997),#6577,.F.);
#6649=ADVANCED_FACE('',(#998,#788),#860,.F.);
#6650=ADVANCED_FACE('',(#999),#6578,.F.);
#6651=ADVANCED_FACE('',(#1000,#789),#861,.F.);
#6652=ADVANCED_FACE('',(#1001),#6579,.F.);
#6653=ADVANCED_FACE('',(#1002),#759,.F.);
#6654=ADVANCED_FACE('',(#1003),#6580,.T.);
#6655=ADVANCED_FACE('',(#1004,#790),#862,.T.);
#6656=ADVANCED_FACE('',(#1005),#667,.T.);
#6657=ADVANCED_FACE('',(#1006,#791),#863,.T.);
#6658=ADVANCED_FACE('',(#1007),#864,.T.);
#6659=ADVANCED_FACE('',(#1008),#668,.T.);
#6660=ADVANCED_FACE('',(#1009),#865,.T.);
#6661=ADVANCED_FACE('',(#1010),#669,.T.);
#6662=ADVANCED_FACE('',(#1011),#866,.T.);
#6663=ADVANCED_FACE('',(#1012),#670,.T.);
#6664=ADVANCED_FACE('',(#1013),#867,.T.);
#6665=ADVANCED_FACE('',(#1014),#671,.T.);
#6666=ADVANCED_FACE('',(#1015),#6581,.T.);
#6667=ADVANCED_FACE('',(#1016,#792),#868,.T.);
#6668=ADVANCED_FACE('',(#1017),#6582,.T.);
#6669=ADVANCED_FACE('',(#1018),#869,.F.);
#6670=ADVANCED_FACE('',(#1019),#672,.T.);
#6671=ADVANCED_FACE('',(#1020),#870,.T.);
#6672=ADVANCED_FACE('',(#1021),#673,.T.);
#6673=ADVANCED_FACE('',(#1022),#871,.T.);
#6674=ADVANCED_FACE('',(#1023),#674,.T.);
#6675=ADVANCED_FACE('',(#1024),#872,.T.);
#6676=ADVANCED_FACE('',(#1025),#675,.T.);
#6677=ADVANCED_FACE('',(#1026),#873,.T.);
#6678=ADVANCED_FACE('',(#1027,#793),#874,.T.);
#6679=ADVANCED_FACE('',(#1028),#676,.F.);
#6680=ADVANCED_FACE('',(#1029),#875,.T.);
#6681=ADVANCED_FACE('',(#1030),#677,.F.);
#6682=ADVANCED_FACE('',(#1031),#876,.T.);
#6683=ADVANCED_FACE('',(#1032),#678,.F.);
#6684=ADVANCED_FACE('',(#1033),#877,.T.);
#6685=ADVANCED_FACE('',(#1034),#679,.F.);
#6686=ADVANCED_FACE('',(#1035),#878,.T.);
#6687=ADVANCED_FACE('',(#1036,#794),#879,.F.);
#6688=ADVANCED_FACE('',(#1037),#6583,.F.);
#6689=ADVANCED_FACE('',(#1038),#880,.F.);
#6690=ADVANCED_FACE('',(#1039),#6584,.F.);
#6691=ADVANCED_FACE('',(#1040,#795),#881,.F.);
#6692=ADVANCED_FACE('',(#1041,#796),#882,.F.);
#6693=ADVANCED_FACE('',(#1042),#6585,.F.);
#6694=ADVANCED_FACE('',(#1043),#6586,.F.);
#6695=ADVANCED_FACE('',(#1044),#883,.T.);
#6696=ADVANCED_FACE('',(#1045),#6587,.T.);
#6697=ADVANCED_FACE('',(#1046,#797),#884,.T.);
#6698=ADVANCED_FACE('',(#1047),#6588,.T.);
#6699=ADVANCED_FACE('',(#1048),#885,.T.);
#6700=ADVANCED_FACE('',(#1049),#680,.T.);
#6701=ADVANCED_FACE('',(#1050),#681,.F.);
#6702=ADVANCED_FACE('',(#1051),#6589,.F.);
#6703=ADVANCED_FACE('',(#1052),#682,.F.);
#6704=ADVANCED_FACE('',(#1053),#6590,.F.);
#6705=ADVANCED_FACE('',(#1054),#683,.F.);
#6706=ADVANCED_FACE('',(#1055,#798),#6591,.F.);
#6707=ADVANCED_FACE('',(#1056,#799),#886,.T.);
#6708=ADVANCED_FACE('',(#1057),#684,.F.);
#6709=ADVANCED_FACE('',(#1058,#800),#887,.T.);
#6710=ADVANCED_FACE('',(#1059),#685,.T.);
#6711=ADVANCED_FACE('',(#1060,#801),#6592,.T.);
#6712=ADVANCED_FACE('',(#1061),#686,.T.);
#6713=ADVANCED_FACE('',(#1062),#687,.T.);
#6714=ADVANCED_FACE('',(#1063),#688,.T.);
#6715=ADVANCED_FACE('',(#1064),#689,.T.);
#6716=ADVANCED_FACE('',(#1065),#690,.T.);
#6717=ADVANCED_FACE('',(#1066),#691,.T.);
#6718=ADVANCED_FACE('',(#1067),#692,.T.);
#6719=ADVANCED_FACE('',(#1068),#693,.T.);
#6720=ADVANCED_FACE('',(#1069),#694,.T.);
#6721=ADVANCED_FACE('',(#1070),#695,.T.);
#6722=ADVANCED_FACE('',(#1071),#696,.T.);
#6723=ADVANCED_FACE('',(#1072),#697,.T.);
#6724=ADVANCED_FACE('',(#1073),#698,.T.);
#6725=ADVANCED_FACE('',(#1074),#699,.T.);
#6726=ADVANCED_FACE('',(#1075),#700,.T.);
#6727=ADVANCED_FACE('',(#1076),#701,.T.);
#6728=ADVANCED_FACE('',(#1077),#702,.T.);
#6729=ADVANCED_FACE('',(#1078),#703,.T.);
#6730=ADVANCED_FACE('',(#1079),#704,.T.);
#6731=ADVANCED_FACE('',(#1080),#705,.T.);
#6732=ADVANCED_FACE('',(#1081),#6593,.T.);
#6733=ADVANCED_FACE('',(#1082),#706,.T.);
#6734=ADVANCED_FACE('',(#1083),#93,.F.);
#6735=ADVANCED_FACE('',(#1084),#94,.F.);
#6736=ADVANCED_FACE('',(#1085),#95,.F.);
#6737=ADVANCED_FACE('',(#1086),#96,.F.);
#6738=ADVANCED_FACE('',(#1087),#97,.F.);
#6739=ADVANCED_FACE('',(#1088),#98,.F.);
#6740=ADVANCED_FACE('',(#1089),#99,.F.);
#6741=ADVANCED_FACE('',(#1090),#100,.F.);
#6742=ADVANCED_FACE('',(#1091),#101,.F.);
#6743=ADVANCED_FACE('',(#1092),#102,.F.);
#6744=ADVANCED_FACE('',(#1093),#103,.F.);
#6745=ADVANCED_FACE('',(#1094),#104,.F.);
#6746=ADVANCED_FACE('',(#1095),#105,.F.);
#6747=ADVANCED_FACE('',(#1096),#106,.F.);
#6748=ADVANCED_FACE('',(#1097),#107,.F.);
#6749=ADVANCED_FACE('',(#1098),#108,.F.);
#6750=ADVANCED_FACE('',(#1099),#109,.F.);
#6751=ADVANCED_FACE('',(#1100),#110,.F.);
#6752=ADVANCED_FACE('',(#1101),#111,.F.);
#6753=ADVANCED_FACE('',(#1102),#112,.F.);
#6754=ADVANCED_FACE('',(#1103),#113,.F.);
#6755=ADVANCED_FACE('',(#1104),#888,.T.);
#6756=ADVANCED_FACE('',(#1105),#707,.T.);
#6757=ADVANCED_FACE('',(#1106),#114,.F.);
#6758=ADVANCED_FACE('',(#1107),#889,.T.);
#6759=ADVANCED_FACE('',(#1108),#115,.F.);
#6760=ADVANCED_FACE('',(#1109),#890,.T.);
#6761=ADVANCED_FACE('',(#1110),#116,.F.);
#6762=ADVANCED_FACE('',(#1111),#891,.T.);
#6763=ADVANCED_FACE('',(#1112),#117,.F.);
#6764=ADVANCED_FACE('',(#1113),#892,.T.);
#6765=ADVANCED_FACE('',(#1114),#118,.F.);
#6766=ADVANCED_FACE('',(#1115),#893,.T.);
#6767=ADVANCED_FACE('',(#1116),#119,.F.);
#6768=ADVANCED_FACE('',(#1117),#894,.T.);
#6769=ADVANCED_FACE('',(#1118),#120,.F.);
#6770=ADVANCED_FACE('',(#1119),#895,.T.);
#6771=ADVANCED_FACE('',(#1120),#121,.F.);
#6772=ADVANCED_FACE('',(#1121),#896,.T.);
#6773=ADVANCED_FACE('',(#1122),#122,.F.);
#6774=ADVANCED_FACE('',(#1123),#897,.T.);
#6775=ADVANCED_FACE('',(#1124),#123,.F.);
#6776=ADVANCED_FACE('',(#1125),#898,.T.);
#6777=ADVANCED_FACE('',(#1126),#124,.F.);
#6778=ADVANCED_FACE('',(#1127),#899,.T.);
#6779=ADVANCED_FACE('',(#1128),#125,.F.);
#6780=ADVANCED_FACE('',(#1129),#900,.T.);
#6781=ADVANCED_FACE('',(#1130),#126,.F.);
#6782=ADVANCED_FACE('',(#1131),#901,.T.);
#6783=ADVANCED_FACE('',(#1132),#127,.F.);
#6784=ADVANCED_FACE('',(#1133),#902,.T.);
#6785=ADVANCED_FACE('',(#1134),#128,.F.);
#6786=ADVANCED_FACE('',(#1135),#903,.T.);
#6787=ADVANCED_FACE('',(#1136),#129,.F.);
#6788=ADVANCED_FACE('',(#1137),#904,.T.);
#6789=ADVANCED_FACE('',(#1138),#130,.F.);
#6790=ADVANCED_FACE('',(#1139),#905,.T.);
#6791=ADVANCED_FACE('',(#1140),#131,.F.);
#6792=ADVANCED_FACE('',(#1141),#906,.T.);
#6793=ADVANCED_FACE('',(#1142),#132,.F.);
#6794=ADVANCED_FACE('',(#1143),#907,.T.);
#6795=ADVANCED_FACE('',(#1144,#802),#908,.T.);
#6796=ADVANCED_FACE('',(#1145),#708,.F.);
#6797=ADVANCED_FACE('',(#1146),#6594,.F.);
#6798=ADVANCED_FACE('',(#1147),#709,.F.);
#6799=ADVANCED_FACE('',(#1148),#6595,.F.);
#6800=ADVANCED_FACE('',(#1149),#710,.F.);
#6801=ADVANCED_FACE('',(#1150,#803),#6596,.F.);
#6802=ADVANCED_FACE('',(#1151,#804),#909,.T.);
#6803=ADVANCED_FACE('',(#1152),#711,.F.);
#6804=ADVANCED_FACE('',(#1153,#805),#910,.T.);
#6805=ADVANCED_FACE('',(#1154),#712,.T.);
#6806=ADVANCED_FACE('',(#1155,#806),#6597,.T.);
#6807=ADVANCED_FACE('',(#1156),#713,.T.);
#6808=ADVANCED_FACE('',(#1157),#714,.T.);
#6809=ADVANCED_FACE('',(#1158),#715,.T.);
#6810=ADVANCED_FACE('',(#1159),#716,.T.);
#6811=ADVANCED_FACE('',(#1160),#717,.T.);
#6812=ADVANCED_FACE('',(#1161),#718,.T.);
#6813=ADVANCED_FACE('',(#1162),#719,.T.);
#6814=ADVANCED_FACE('',(#1163),#720,.T.);
#6815=ADVANCED_FACE('',(#1164),#721,.T.);
#6816=ADVANCED_FACE('',(#1165),#722,.T.);
#6817=ADVANCED_FACE('',(#1166),#723,.T.);
#6818=ADVANCED_FACE('',(#1167),#724,.T.);
#6819=ADVANCED_FACE('',(#1168),#725,.T.);
#6820=ADVANCED_FACE('',(#1169),#726,.T.);
#6821=ADVANCED_FACE('',(#1170),#727,.T.);
#6822=ADVANCED_FACE('',(#1171),#728,.T.);
#6823=ADVANCED_FACE('',(#1172),#729,.T.);
#6824=ADVANCED_FACE('',(#1173),#730,.T.);
#6825=ADVANCED_FACE('',(#1174),#731,.T.);
#6826=ADVANCED_FACE('',(#1175),#732,.T.);
#6827=ADVANCED_FACE('',(#1176),#6598,.T.);
#6828=ADVANCED_FACE('',(#1177),#733,.T.);
#6829=ADVANCED_FACE('',(#1178),#133,.F.);
#6830=ADVANCED_FACE('',(#1179),#134,.F.);
#6831=ADVANCED_FACE('',(#1180),#135,.F.);
#6832=ADVANCED_FACE('',(#1181),#136,.F.);
#6833=ADVANCED_FACE('',(#1182),#137,.F.);
#6834=ADVANCED_FACE('',(#1183),#138,.F.);
#6835=ADVANCED_FACE('',(#1184),#139,.F.);
#6836=ADVANCED_FACE('',(#1185),#140,.F.);
#6837=ADVANCED_FACE('',(#1186),#141,.F.);
#6838=ADVANCED_FACE('',(#1187),#142,.F.);
#6839=ADVANCED_FACE('',(#1188),#143,.F.);
#6840=ADVANCED_FACE('',(#1189),#144,.F.);
#6841=ADVANCED_FACE('',(#1190),#145,.F.);
#6842=ADVANCED_FACE('',(#1191),#146,.F.);
#6843=ADVANCED_FACE('',(#1192),#147,.F.);
#6844=ADVANCED_FACE('',(#1193),#148,.F.);
#6845=ADVANCED_FACE('',(#1194),#149,.F.);
#6846=ADVANCED_FACE('',(#1195),#150,.F.);
#6847=ADVANCED_FACE('',(#1196),#151,.F.);
#6848=ADVANCED_FACE('',(#1197),#152,.F.);
#6849=ADVANCED_FACE('',(#1198),#153,.F.);
#6850=ADVANCED_FACE('',(#1199),#911,.T.);
#6851=ADVANCED_FACE('',(#1200),#734,.T.);
#6852=ADVANCED_FACE('',(#1201),#154,.F.);
#6853=ADVANCED_FACE('',(#1202),#912,.T.);
#6854=ADVANCED_FACE('',(#1203),#155,.F.);
#6855=ADVANCED_FACE('',(#1204),#913,.T.);
#6856=ADVANCED_FACE('',(#1205),#156,.F.);
#6857=ADVANCED_FACE('',(#1206),#914,.T.);
#6858=ADVANCED_FACE('',(#1207),#157,.F.);
#6859=ADVANCED_FACE('',(#1208),#915,.T.);
#6860=ADVANCED_FACE('',(#1209),#158,.F.);
#6861=ADVANCED_FACE('',(#1210),#916,.T.);
#6862=ADVANCED_FACE('',(#1211),#159,.F.);
#6863=ADVANCED_FACE('',(#1212),#917,.T.);
#6864=ADVANCED_FACE('',(#1213),#160,.F.);
#6865=ADVANCED_FACE('',(#1214),#918,.T.);
#6866=ADVANCED_FACE('',(#1215),#161,.F.);
#6867=ADVANCED_FACE('',(#1216),#919,.T.);
#6868=ADVANCED_FACE('',(#1217),#162,.F.);
#6869=ADVANCED_FACE('',(#1218),#920,.T.);
#6870=ADVANCED_FACE('',(#1219),#163,.F.);
#6871=ADVANCED_FACE('',(#1220),#921,.T.);
#6872=ADVANCED_FACE('',(#1221),#164,.F.);
#6873=ADVANCED_FACE('',(#1222),#922,.T.);
#6874=ADVANCED_FACE('',(#1223),#165,.F.);
#6875=ADVANCED_FACE('',(#1224),#923,.T.);
#6876=ADVANCED_FACE('',(#1225),#166,.F.);
#6877=ADVANCED_FACE('',(#1226),#924,.T.);
#6878=ADVANCED_FACE('',(#1227),#167,.F.);
#6879=ADVANCED_FACE('',(#1228),#925,.T.);
#6880=ADVANCED_FACE('',(#1229),#168,.F.);
#6881=ADVANCED_FACE('',(#1230),#926,.T.);
#6882=ADVANCED_FACE('',(#1231),#169,.F.);
#6883=ADVANCED_FACE('',(#1232),#927,.T.);
#6884=ADVANCED_FACE('',(#1233),#170,.F.);
#6885=ADVANCED_FACE('',(#1234),#928,.T.);
#6886=ADVANCED_FACE('',(#1235),#171,.F.);
#6887=ADVANCED_FACE('',(#1236),#929,.T.);
#6888=ADVANCED_FACE('',(#1237),#172,.F.);
#6889=ADVANCED_FACE('',(#1238),#930,.T.);
#6890=ADVANCED_FACE('',(#1239,#807),#931,.T.);
#6891=ADVANCED_FACE('',(#1240),#932,.F.);
#6892=ADVANCED_FACE('',(#1241),#933,.F.);
#6893=ADVANCED_FACE('',(#1242),#934,.F.);
#6894=ADVANCED_FACE('',(#1243),#935,.F.);
#6895=ADVANCED_FACE('',(#1244),#936,.F.);
#6896=ADVANCED_FACE('',(#1245),#937,.F.);
#6897=ADVANCED_FACE('',(#1246),#735,.F.);
#6898=ADVANCED_FACE('',(#1247),#6599,.F.);
#6899=ADVANCED_FACE('',(#1248),#6600,.F.);
#6900=ADVANCED_FACE('',(#1249),#736,.F.);
#6901=ADVANCED_FACE('',(#1250,#808),#938,.T.);
#6902=ADVANCED_FACE('',(#1251),#737,.T.);
#6903=ADVANCED_FACE('',(#1252,#809),#6601,.T.);
#6904=ADVANCED_FACE('',(#1253),#738,.T.);
#6905=ADVANCED_FACE('',(#1254,#810),#939,.T.);
#6906=ADVANCED_FACE('',(#1255),#940,.F.);
#6907=ADVANCED_FACE('',(#1256),#941,.F.);
#6908=ADVANCED_FACE('',(#1257),#942,.F.);
#6909=ADVANCED_FACE('',(#1258),#943,.F.);
#6910=ADVANCED_FACE('',(#1259),#944,.F.);
#6911=ADVANCED_FACE('',(#1260),#945,.F.);
#6912=ADVANCED_FACE('',(#1261),#739,.F.);
#6913=ADVANCED_FACE('',(#1262),#6602,.F.);
#6914=ADVANCED_FACE('',(#1263),#6603,.F.);
#6915=ADVANCED_FACE('',(#1264),#740,.F.);
#6916=ADVANCED_FACE('',(#1265,#811),#946,.T.);
#6917=ADVANCED_FACE('',(#1266),#741,.T.);
#6918=ADVANCED_FACE('',(#1267,#812),#6604,.T.);
#6919=ADVANCED_FACE('',(#1268),#742,.T.);
#6920=ADVANCED_FACE('',(#1269,#813),#947,.T.);
#6921=ADVANCED_FACE('',(#1270,#814,#815),#83,.T.);
#6922=ADVANCED_FACE('',(#1271),#743,.F.);
#6923=ADVANCED_FACE('',(#1272),#760,.F.);
#6924=ADVANCED_FACE('',(#1273),#6605,.T.);
#6925=ADVANCED_FACE('',(#1274),#761,.F.);
#6926=ADVANCED_FACE('',(#1275,#816,#817),#84,.T.);
#6927=ADVANCED_FACE('',(#1276),#762,.F.);
#6928=ADVANCED_FACE('',(#1277),#763,.F.);
#6929=ADVANCED_FACE('',(#1278,#818,#819),#85,.T.);
#6930=ADVANCED_FACE('',(#1279),#764,.F.);
#6931=ADVANCED_FACE('',(#1280),#765,.F.);
#6932=ADVANCED_FACE('',(#1281,#820,#821),#86,.T.);
#6933=ADVANCED_FACE('',(#1282),#766,.F.);
#6934=ADVANCED_FACE('',(#1283),#767,.F.);
#6935=ADVANCED_FACE('',(#1284,#822,#823),#87,.T.);
#6936=ADVANCED_FACE('',(#1285),#768,.F.);
#6937=ADVANCED_FACE('',(#1286),#769,.F.);
#6938=ADVANCED_FACE('',(#1287,#824,#825),#88,.T.);
#6939=ADVANCED_FACE('',(#1288),#770,.F.);
#6940=ADVANCED_FACE('',(#1289),#771,.F.);
#6941=ADVANCED_FACE('',(#1290,#826,#827),#89,.T.);
#6942=ADVANCED_FACE('',(#1291),#772,.F.);
#6943=ADVANCED_FACE('',(#1292),#773,.F.);
#6944=ADVANCED_FACE('',(#1293,#828,#829),#90,.T.);
#6945=ADVANCED_FACE('',(#1294),#774,.F.);
#6946=ADVANCED_FACE('',(#1295),#775,.F.);
#6947=ADVANCED_FACE('',(#1296,#830,#831),#91,.T.);
#6948=ADVANCED_FACE('',(#1297),#6606,.F.);
#6949=ADVANCED_FACE('',(#1298),#776,.F.);
#6950=ADVANCED_FACE('',(#1299),#6607,.T.);
#6951=ADVANCED_FACE('',(#1300),#777,.F.);
#6952=ADVANCED_FACE('',(#1301,#832,#833),#92,.T.);
#6953=ADVANCED_FACE('',(#1302),#778,.F.);
#6954=ADVANCED_FACE('',(#1303,#834),#948,.T.);
#6955=ADVANCED_FACE('',(#1304),#744,.T.);
#6956=ADVANCED_FACE('',(#1305),#6608,.T.);
#6957=ADVANCED_FACE('',(#1306),#745,.T.);
#6958=ADVANCED_FACE('',(#1307,#835),#949,.T.);
#6959=ADVANCED_FACE('',(#1308),#6609,.F.);
#6960=ADVANCED_FACE('',(#1309),#779,.F.);
#6961=ADVANCED_FACE('',(#1310,#836),#950,.T.);
#6962=ADVANCED_FACE('',(#1311),#746,.F.);
#6963=ADVANCED_FACE('',(#1312),#6610,.F.);
#6964=ADVANCED_FACE('',(#1313),#747,.F.);
#6965=ADVANCED_FACE('',(#1314,#837),#951,.T.);
#6966=ADVANCED_FACE('',(#1315,#838),#952,.T.);
#6967=ADVANCED_FACE('',(#1316),#748,.T.);
#6968=ADVANCED_FACE('',(#1317,#839),#953,.T.);
#6969=ADVANCED_FACE('',(#1318),#749,.F.);
#6970=ADVANCED_FACE('',(#1319,#840),#954,.T.);
#6971=ADVANCED_FACE('',(#1320),#750,.T.);
#6972=ADVANCED_FACE('',(#1321),#6611,.T.);
#6973=ADVANCED_FACE('',(#1322),#751,.T.);
#6974=ADVANCED_FACE('',(#1323,#841),#955,.T.);
#6975=ADVANCED_FACE('',(#1324),#752,.F.);
#6976=ADVANCED_FACE('',(#1325,#842),#956,.T.);
#6977=ADVANCED_FACE('',(#1326),#753,.T.);
#6978=ADVANCED_FACE('',(#1327,#843),#957,.T.);
#6979=ADVANCED_FACE('',(#1328),#754,.F.);
#6980=ADVANCED_FACE('',(#1329),#6612,.F.);
#6981=ADVANCED_FACE('',(#1330),#755,.F.);
#6982=ADVANCED_FACE('',(#1331),#6613,.T.);
#6983=ADVANCED_FACE('',(#1332,#844),#958,.T.);
#6984=ADVANCED_FACE('',(#1333),#6614,.F.);
#6985=ADVANCED_FACE('',(#1334,#845),#959,.T.);
#6986=ADVANCED_FACE('',(#1335),#6615,.T.);
#6987=ADVANCED_FACE('',(#1336),#6616,.T.);
#6988=ADVANCED_FACE('',(#1337),#6617,.T.);
#6989=ADVANCED_FACE('',(#1338),#6618,.T.);
#6990=ADVANCED_FACE('',(#1339),#6619,.T.);
#6991=ADVANCED_FACE('',(#1340),#6620,.T.);
#6992=ADVANCED_FACE('',(#1341),#6621,.T.);
#6993=ADVANCED_FACE('',(#1342),#6622,.T.);
#6994=ADVANCED_FACE('',(#1343),#6623,.T.);
#6995=ADVANCED_FACE('',(#1344),#960,.F.);
#6996=ADVANCED_FACE('',(#1345),#173,.F.);
#6997=ADVANCED_FACE('',(#1346),#961,.T.);
#6998=ADVANCED_FACE('',(#1347),#6624,.T.);
#6999=ADVANCED_FACE('',(#1348),#174,.F.);
#7000=ADVANCED_FACE('',(#1349),#756,.F.);
#7001=ADVANCED_FACE('',(#1350),#962,.F.);
#7002=ADVANCED_FACE('',(#1351),#963,.F.);
#7003=ADVANCED_FACE('',(#1352),#964,.F.);
#7004=ADVANCED_FACE('',(#1353),#965,.F.);
#7005=ADVANCED_FACE('',(#1354),#966,.F.);
#7006=ADVANCED_FACE('',(#1355),#967,.F.);
#7007=ADVANCED_FACE('',(#1356,#846),#968,.T.);
#7008=ADVANCED_FACE('',(#1357),#969,.T.);
#7009=ADVANCED_FACE('',(#1358),#757,.T.);
#7010=ADVANCED_FACE('',(#1359),#6625,.T.);
#7011=ADVANCED_FACE('',(#1360),#758,.T.);
#7012=ADVANCED_FACE('',(#1361,#847),#970,.T.);
#7013=ADVANCED_FACE('',(#1362),#6626,.F.);
#7014=ADVANCED_FACE('',(#1363),#6627,.F.);
#7015=ADVANCED_FACE('',(#1364),#6628,.T.);
#7016=ADVANCED_FACE('',(#1365,#848,#849),#971,.T.);
#7017=ADVANCED_FACE('',(#1366),#972,.T.);
#7018=ADVANCED_FACE('',(#1367),#973,.T.);
#7019=ADVANCED_FACE('',(#1368),#974,.T.);
#7020=ADVANCED_FACE('',(#1369),#975,.T.);
#7021=ADVANCED_FACE('',(#1370),#976,.T.);
#7022=ADVANCED_FACE('',(#1371),#977,.T.);
#7023=ADVANCED_FACE('',(#1372,#850,#851),#978,.T.);
#7024=ADVANCED_FACE('',(#1373),#6629,.F.);
#7025=CLOSED_SHELL('',(#6630,#6631,#6632,#6633,#6634,#6635,#6636,#6637,
#6638,#6639,#6640,#6641,#6642,#6643,#6644,#6645,#6646,#6647,#6648,#6649,
#6650,#6651,#6652,#6653,#6654,#6655,#6656,#6657,#6658,#6659,#6660,#6661,
#6662,#6663,#6664,#6665,#6666,#6667,#6668,#6669,#6670,#6671,#6672,#6673,
#6674,#6675,#6676,#6677,#6678,#6679,#6680,#6681,#6682,#6683,#6684,#6685,
#6686,#6687,#6688,#6689,#6690,#6691,#6692,#6693,#6694,#6695,#6696,#6697,
#6698,#6699));
#7026=CLOSED_SHELL('',(#6700,#6701,#6702,#6703,#6704,#6705,#6706,#6707,
#6708,#6709,#6710,#6711,#6712,#6713,#6714,#6715,#6716,#6717,#6718,#6719,
#6720,#6721,#6722,#6723,#6724,#6725,#6726,#6727,#6728,#6729,#6730,#6731,
#6732,#6733,#6734,#6735,#6736,#6737,#6738,#6739,#6740,#6741,#6742,#6743,
#6744,#6745,#6746,#6747,#6748,#6749,#6750,#6751,#6752,#6753,#6754,#6755,
#6756,#6757,#6758,#6759,#6760,#6761,#6762,#6763,#6764,#6765,#6766,#6767,
#6768,#6769,#6770,#6771,#6772,#6773,#6774,#6775,#6776,#6777,#6778,#6779,
#6780,#6781,#6782,#6783,#6784,#6785,#6786,#6787,#6788,#6789,#6790,#6791,
#6792,#6793,#6794,#6795));
#7027=CLOSED_SHELL('',(#6796,#6797,#6798,#6799,#6800,#6801,#6802,#6803,
#6804,#6805,#6806,#6807,#6808,#6809,#6810,#6811,#6812,#6813,#6814,#6815,
#6816,#6817,#6818,#6819,#6820,#6821,#6822,#6823,#6824,#6825,#6826,#6827,
#6828,#6829,#6830,#6831,#6832,#6833,#6834,#6835,#6836,#6837,#6838,#6839,
#6840,#6841,#6842,#6843,#6844,#6845,#6846,#6847,#6848,#6849,#6850,#6851,
#6852,#6853,#6854,#6855,#6856,#6857,#6858,#6859,#6860,#6861,#6862,#6863,
#6864,#6865,#6866,#6867,#6868,#6869,#6870,#6871,#6872,#6873,#6874,#6875,
#6876,#6877,#6878,#6879,#6880,#6881,#6882,#6883,#6884,#6885,#6886,#6887,
#6888,#6889,#6890));
#7028=CLOSED_SHELL('',(#6891,#6892,#6893,#6894,#6895,#6896,#6897,#6898,
#6899,#6900,#6901,#6902,#6903,#6904,#6905));
#7029=CLOSED_SHELL('',(#6906,#6907,#6908,#6909,#6910,#6911,#6912,#6913,
#6914,#6915,#6916,#6917,#6918,#6919,#6920));
#7030=CLOSED_SHELL('',(#6921,#6922,#6923,#6924,#6925,#6926,#6927,#6928,
#6929,#6930,#6931,#6932,#6933,#6934,#6935,#6936,#6937,#6938,#6939,#6940,
#6941,#6942,#6943,#6944,#6945,#6946,#6947,#6948,#6949,#6950,#6951,#6952,
#6953,#6954,#6955,#6956,#6957,#6958,#6959,#6960,#6961,#6962,#6963,#6964,
#6965));
#7031=CLOSED_SHELL('',(#6966,#6967,#6968,#6969,#6970,#6971,#6972,#6973,
#6974,#6975,#6976,#6977,#6978,#6979,#6980,#6981));
#7032=CLOSED_SHELL('',(#6982,#6983,#6984,#6985));
#7033=CLOSED_SHELL('',(#6986,#6987,#6988,#6989,#6990,#6991,#6992,#6993,
#6994,#6995,#6996,#6997,#6998,#6999,#7000,#7001,#7002,#7003,#7004,#7005,
#7006,#7007,#7008,#7009,#7010,#7011,#7012));
#7034=CLOSED_SHELL('',(#7013,#7014,#7015,#7016,#7017,#7018,#7019,#7020,
#7021,#7022,#7023,#7024));
#7035=DERIVED_UNIT_ELEMENT(#7055,1.);
#7036=DERIVED_UNIT_ELEMENT(#23256,-3.);
#7037=DERIVED_UNIT_ELEMENT(#7055,1.);
#7038=DERIVED_UNIT_ELEMENT(#23256,-3.);
#7039=DERIVED_UNIT_ELEMENT(#7055,1.);
#7040=DERIVED_UNIT_ELEMENT(#23256,-3.);
#7041=DERIVED_UNIT_ELEMENT(#7055,1.);
#7042=DERIVED_UNIT_ELEMENT(#23256,-3.);
#7043=DERIVED_UNIT_ELEMENT(#7055,1.);
#7044=DERIVED_UNIT_ELEMENT(#23256,-3.);
#7045=DERIVED_UNIT_ELEMENT(#7055,1.);
#7046=DERIVED_UNIT_ELEMENT(#23256,-3.);
#7047=DERIVED_UNIT_ELEMENT(#7055,1.);
#7048=DERIVED_UNIT_ELEMENT(#23256,-3.);
#7049=DERIVED_UNIT_ELEMENT(#7055,1.);
#7050=DERIVED_UNIT_ELEMENT(#23256,-3.);
#7051=DERIVED_UNIT_ELEMENT(#7055,1.);
#7052=DERIVED_UNIT_ELEMENT(#23256,-3.);
#7053=DERIVED_UNIT_ELEMENT(#7055,1.);
#7054=DERIVED_UNIT_ELEMENT(#23256,-3.);
#7055=(
MASS_UNIT()
NAMED_UNIT(*)
SI_UNIT(.KILO.,.GRAM.)
);
#7056=DERIVED_UNIT((#7035,#7036));
#7057=DERIVED_UNIT((#7037,#7038));
#7058=DERIVED_UNIT((#7039,#7040));
#7059=DERIVED_UNIT((#7041,#7042));
#7060=DERIVED_UNIT((#7043,#7044));
#7061=DERIVED_UNIT((#7045,#7046));
#7062=DERIVED_UNIT((#7047,#7048));
#7063=DERIVED_UNIT((#7049,#7050));
#7064=DERIVED_UNIT((#7051,#7052));
#7065=DERIVED_UNIT((#7053,#7054));
#7066=MEASURE_REPRESENTATION_ITEM('density measure',
POSITIVE_RATIO_MEASURE(7850.),#7056);
#7067=MEASURE_REPRESENTATION_ITEM('density measure',
POSITIVE_RATIO_MEASURE(7850.),#7057);
#7068=MEASURE_REPRESENTATION_ITEM('density measure',
POSITIVE_RATIO_MEASURE(7850.),#7058);
#7069=MEASURE_REPRESENTATION_ITEM('density measure',
POSITIVE_RATIO_MEASURE(7850.),#7059);
#7070=MEASURE_REPRESENTATION_ITEM('density measure',
POSITIVE_RATIO_MEASURE(7850.),#7060);
#7071=MEASURE_REPRESENTATION_ITEM('density measure',
POSITIVE_RATIO_MEASURE(7850.),#7061);
#7072=MEASURE_REPRESENTATION_ITEM('density measure',
POSITIVE_RATIO_MEASURE(7850.),#7062);
#7073=MEASURE_REPRESENTATION_ITEM('density measure',
POSITIVE_RATIO_MEASURE(7850.),#7063);
#7074=MEASURE_REPRESENTATION_ITEM('density measure',
POSITIVE_RATIO_MEASURE(7850.),#7064);
#7075=MEASURE_REPRESENTATION_ITEM('density measure',
POSITIVE_RATIO_MEASURE(7850.),#7065);
#7076=PROPERTY_DEFINITION_REPRESENTATION(#7126,#7096);
#7077=PROPERTY_DEFINITION_REPRESENTATION(#7127,#7097);
#7078=PROPERTY_DEFINITION_REPRESENTATION(#7128,#7098);
#7079=PROPERTY_DEFINITION_REPRESENTATION(#7129,#7099);
#7080=PROPERTY_DEFINITION_REPRESENTATION(#7130,#7100);
#7081=PROPERTY_DEFINITION_REPRESENTATION(#7131,#7101);
#7082=PROPERTY_DEFINITION_REPRESENTATION(#7132,#7102);
#7083=PROPERTY_DEFINITION_REPRESENTATION(#7133,#7103);
#7084=PROPERTY_DEFINITION_REPRESENTATION(#7134,#7104);
#7085=PROPERTY_DEFINITION_REPRESENTATION(#7135,#7105);
#7086=PROPERTY_DEFINITION_REPRESENTATION(#7136,#7106);
#7087=PROPERTY_DEFINITION_REPRESENTATION(#7137,#7107);
#7088=PROPERTY_DEFINITION_REPRESENTATION(#7138,#7108);
#7089=PROPERTY_DEFINITION_REPRESENTATION(#7139,#7109);
#7090=PROPERTY_DEFINITION_REPRESENTATION(#7140,#7110);
#7091=PROPERTY_DEFINITION_REPRESENTATION(#7141,#7111);
#7092=PROPERTY_DEFINITION_REPRESENTATION(#7142,#7112);
#7093=PROPERTY_DEFINITION_REPRESENTATION(#7143,#7113);
#7094=PROPERTY_DEFINITION_REPRESENTATION(#7144,#7114);
#7095=PROPERTY_DEFINITION_REPRESENTATION(#7145,#7115);
#7096=REPRESENTATION('material name',(#7116),#23244);
#7097=REPRESENTATION('density',(#7066),#23244);
#7098=REPRESENTATION('material name',(#7117),#23245);
#7099=REPRESENTATION('density',(#7067),#23245);
#7100=REPRESENTATION('material name',(#7118),#23246);
#7101=REPRESENTATION('density',(#7068),#23246);
#7102=REPRESENTATION('material name',(#7119),#23247);
#7103=REPRESENTATION('density',(#7069),#23247);
#7104=REPRESENTATION('material name',(#7120),#23248);
#7105=REPRESENTATION('density',(#7070),#23248);
#7106=REPRESENTATION('material name',(#7121),#23249);
#7107=REPRESENTATION('density',(#7071),#23249);
#7108=REPRESENTATION('material name',(#7122),#23250);
#7109=REPRESENTATION('density',(#7072),#23250);
#7110=REPRESENTATION('material name',(#7123),#23251);
#7111=REPRESENTATION('density',(#7073),#23251);
#7112=REPRESENTATION('material name',(#7124),#23252);
#7113=REPRESENTATION('density',(#7074),#23252);
#7114=REPRESENTATION('material name',(#7125),#23253);
#7115=REPRESENTATION('density',(#7075),#23253);
#7116=DESCRIPTIVE_REPRESENTATION_ITEM('Steel','Steel');
#7117=DESCRIPTIVE_REPRESENTATION_ITEM('Steel','Steel');
#7118=DESCRIPTIVE_REPRESENTATION_ITEM('Steel','Steel');
#7119=DESCRIPTIVE_REPRESENTATION_ITEM('Steel','Steel');
#7120=DESCRIPTIVE_REPRESENTATION_ITEM('Steel','Steel');
#7121=DESCRIPTIVE_REPRESENTATION_ITEM('Steel','Steel');
#7122=DESCRIPTIVE_REPRESENTATION_ITEM('Steel','Steel');
#7123=DESCRIPTIVE_REPRESENTATION_ITEM('Steel','Steel');
#7124=DESCRIPTIVE_REPRESENTATION_ITEM('Steel','Steel');
#7125=DESCRIPTIVE_REPRESENTATION_ITEM('Steel','Steel');
#7126=PROPERTY_DEFINITION('material property','material name',#23312);
#7127=PROPERTY_DEFINITION('material property','density of part',#23312);
#7128=PROPERTY_DEFINITION('material property','material name',#23313);
#7129=PROPERTY_DEFINITION('material property','density of part',#23313);
#7130=PROPERTY_DEFINITION('material property','material name',#23314);
#7131=PROPERTY_DEFINITION('material property','density of part',#23314);
#7132=PROPERTY_DEFINITION('material property','material name',#23315);
#7133=PROPERTY_DEFINITION('material property','density of part',#23315);
#7134=PROPERTY_DEFINITION('material property','material name',#23316);
#7135=PROPERTY_DEFINITION('material property','density of part',#23316);
#7136=PROPERTY_DEFINITION('material property','material name',#23317);
#7137=PROPERTY_DEFINITION('material property','density of part',#23317);
#7138=PROPERTY_DEFINITION('material property','material name',#23318);
#7139=PROPERTY_DEFINITION('material property','density of part',#23318);
#7140=PROPERTY_DEFINITION('material property','material name',#23319);
#7141=PROPERTY_DEFINITION('material property','density of part',#23319);
#7142=PROPERTY_DEFINITION('material property','material name',#23320);
#7143=PROPERTY_DEFINITION('material property','density of part',#23320);
#7144=PROPERTY_DEFINITION('material property','material name',#23321);
#7145=PROPERTY_DEFINITION('material property','density of part',#23321);
#7146=AXIS2_PLACEMENT_3D('',#9460,#7831,#7832);
#7147=AXIS2_PLACEMENT_3D('',#9461,#7833,#7834);
#7148=AXIS2_PLACEMENT_3D('',#9462,#7835,#7836);
#7149=AXIS2_PLACEMENT_3D('',#9464,#7837,#7838);
#7150=AXIS2_PLACEMENT_3D('',#9467,#7840,#7841);
#7151=AXIS2_PLACEMENT_3D('',#9468,#7842,#7843);
#7152=AXIS2_PLACEMENT_3D('',#9470,#7844,#7845);
#7153=AXIS2_PLACEMENT_3D('',#9471,#7846,#7847);
#7154=AXIS2_PLACEMENT_3D('',#9474,#7849,#7850);
#7155=AXIS2_PLACEMENT_3D('',#9475,#7851,#7852);
#7156=AXIS2_PLACEMENT_3D('',#9477,#7853,#7854);
#7157=AXIS2_PLACEMENT_3D('',#9478,#7855,#7856);
#7158=AXIS2_PLACEMENT_3D('',#9481,#7858,#7859);
#7159=AXIS2_PLACEMENT_3D('',#9482,#7860,#7861);
#7160=AXIS2_PLACEMENT_3D('',#9484,#7862,#7863);
#7161=AXIS2_PLACEMENT_3D('',#9485,#7864,#7865);
#7162=AXIS2_PLACEMENT_3D('',#9488,#7867,#7868);
#7163=AXIS2_PLACEMENT_3D('',#9489,#7869,#7870);
#7164=AXIS2_PLACEMENT_3D('',#9491,#7871,#7872);
#7165=AXIS2_PLACEMENT_3D('',#9492,#7873,#7874);
#7166=AXIS2_PLACEMENT_3D('',#9495,#7876,#7877);
#7167=AXIS2_PLACEMENT_3D('',#9496,#7878,#7879);
#7168=AXIS2_PLACEMENT_3D('',#9498,#7880,#7881);
#7169=AXIS2_PLACEMENT_3D('',#9501,#7883,#7884);
#7170=AXIS2_PLACEMENT_3D('',#9502,#7885,#7886);
#7171=AXIS2_PLACEMENT_3D('',#9504,#7887,#7888);
#7172=AXIS2_PLACEMENT_3D('',#9505,#7889,#7890);
#7173=AXIS2_PLACEMENT_3D('',#9508,#7892,#7893);
#7174=AXIS2_PLACEMENT_3D('',#9509,#7894,#7895);
#7175=AXIS2_PLACEMENT_3D('',#9511,#7896,#7897);
#7176=AXIS2_PLACEMENT_3D('',#9512,#7898,#7899);
#7177=AXIS2_PLACEMENT_3D('',#9515,#7901,#7902);
#7178=AXIS2_PLACEMENT_3D('',#9516,#7903,#7904);
#7179=AXIS2_PLACEMENT_3D('',#9518,#7905,#7906);
#7180=AXIS2_PLACEMENT_3D('',#9519,#7907,#7908);
#7181=AXIS2_PLACEMENT_3D('',#9522,#7910,#7911);
#7182=AXIS2_PLACEMENT_3D('',#9523,#7912,#7913);
#7183=AXIS2_PLACEMENT_3D('',#9525,#7914,#7915);
#7184=AXIS2_PLACEMENT_3D('',#9528,#7917,#7918);
#7185=AXIS2_PLACEMENT_3D('',#9529,#7919,#7920);
#7186=AXIS2_PLACEMENT_3D('',#9531,#7921,#7922);
#7187=AXIS2_PLACEMENT_3D('',#9532,#7923,#7924);
#7188=AXIS2_PLACEMENT_3D('',#9535,#7926,#7927);
#7189=AXIS2_PLACEMENT_3D('',#9536,#7928,#7929);
#7190=AXIS2_PLACEMENT_3D('',#9538,#7930,#7931);
#7191=AXIS2_PLACEMENT_3D('',#9539,#7932,#7933);
#7192=AXIS2_PLACEMENT_3D('',#9542,#7935,#7936);
#7193=AXIS2_PLACEMENT_3D('',#9543,#7937,#7938);
#7194=AXIS2_PLACEMENT_3D('',#9545,#7939,#7940);
#7195=AXIS2_PLACEMENT_3D('',#9546,#7941,#7942);
#7196=AXIS2_PLACEMENT_3D('',#9549,#7944,#7945);
#7197=AXIS2_PLACEMENT_3D('',#9550,#7946,#7947);
#7198=AXIS2_PLACEMENT_3D('',#9553,#7948,#7949);
#7199=AXIS2_PLACEMENT_3D('',#9555,#7950,#7951);
#7200=AXIS2_PLACEMENT_3D('',#9556,#7952,#7953);
#7201=AXIS2_PLACEMENT_3D('',#9557,#7954,#7955);
#7202=AXIS2_PLACEMENT_3D('',#9558,#7956,#7957);
#7203=AXIS2_PLACEMENT_3D('',#9562,#7959,#7960);
#7204=AXIS2_PLACEMENT_3D('',#9563,#7961,#7962);
#7205=AXIS2_PLACEMENT_3D('',#9564,#7963,#7964);
#7206=AXIS2_PLACEMENT_3D('',#9569,#7966,#7967);
#7207=AXIS2_PLACEMENT_3D('',#9573,#7969,#7970);
#7208=AXIS2_PLACEMENT_3D('',#9577,#7972,#7973);
#7209=AXIS2_PLACEMENT_3D('',#9580,#7975,#7976);
#7210=AXIS2_PLACEMENT_3D('',#9581,#7977,#7978);
#7211=AXIS2_PLACEMENT_3D('',#9584,#7980,#7981);
#7212=AXIS2_PLACEMENT_3D('',#9585,#7982,#7983);
#7213=AXIS2_PLACEMENT_3D('',#9586,#7984,#7985);
#7214=AXIS2_PLACEMENT_3D('',#9592,#7989,#7990);
#7215=AXIS2_PLACEMENT_3D('',#9594,#7991,#7992);
#7216=AXIS2_PLACEMENT_3D('',#9596,#7994,#7995);
#7217=AXIS2_PLACEMENT_3D('',#9600,#7998,#7999);
#7218=AXIS2_PLACEMENT_3D('',#9602,#8000,#8001);
#7219=AXIS2_PLACEMENT_3D('',#9604,#8003,#8004);
#7220=AXIS2_PLACEMENT_3D('',#9608,#8007,#8008);
#7221=AXIS2_PLACEMENT_3D('',#9610,#8009,#8010);
#7222=AXIS2_PLACEMENT_3D('',#9612,#8012,#8013);
#7223=AXIS2_PLACEMENT_3D('',#9616,#8016,#8017);
#7224=AXIS2_PLACEMENT_3D('',#9617,#8018,#8019);
#7225=AXIS2_PLACEMENT_3D('',#9618,#8020,#8021);
#7226=AXIS2_PLACEMENT_3D('',#9622,#8023,#8024);
#7227=AXIS2_PLACEMENT_3D('',#9624,#8026,#8027);
#7228=AXIS2_PLACEMENT_3D('',#9628,#8030,#8031);
#7229=AXIS2_PLACEMENT_3D('',#9631,#8033,#8034);
#7230=AXIS2_PLACEMENT_3D('',#9632,#8035,#8036);
#7231=AXIS2_PLACEMENT_3D('',#9636,#8039,#8040);
#7232=AXIS2_PLACEMENT_3D('',#9641,#8043,#8044);
#7233=AXIS2_PLACEMENT_3D('',#9642,#8045,#8046);
#7234=AXIS2_PLACEMENT_3D('',#9648,#8050,#8051);
#7235=AXIS2_PLACEMENT_3D('',#9652,#8053,#8054);
#7236=AXIS2_PLACEMENT_3D('',#9653,#8055,#8056);
#7237=AXIS2_PLACEMENT_3D('',#9654,#8057,#8058);
#7238=AXIS2_PLACEMENT_3D('',#9660,#8062,#8063);
#7239=AXIS2_PLACEMENT_3D('',#9663,#8065,#8066);
#7240=AXIS2_PLACEMENT_3D('',#9664,#8067,#8068);
#7241=AXIS2_PLACEMENT_3D('',#9665,#8069,#8070);
#7242=AXIS2_PLACEMENT_3D('',#9669,#8073,#8074);
#7243=AXIS2_PLACEMENT_3D('',#9672,#8076,#8077);
#7244=AXIS2_PLACEMENT_3D('',#9673,#8078,#8079);
#7245=AXIS2_PLACEMENT_3D('',#9675,#8081,#8082);
#7246=AXIS2_PLACEMENT_3D('',#9678,#8083,#8084);
#7247=AXIS2_PLACEMENT_3D('',#9682,#8086,#8087);
#7248=AXIS2_PLACEMENT_3D('',#9686,#8089,#8090);
#7249=AXIS2_PLACEMENT_3D('',#9690,#8092,#8093);
#7250=AXIS2_PLACEMENT_3D('',#9692,#8095,#8096);
#7251=AXIS2_PLACEMENT_3D('',#9696,#8098,#8099);
#7252=AXIS2_PLACEMENT_3D('',#9698,#8101,#8102);
#7253=AXIS2_PLACEMENT_3D('',#9702,#8105,#8106);
#7254=AXIS2_PLACEMENT_3D('',#9705,#8108,#8109);
#7255=AXIS2_PLACEMENT_3D('',#9706,#8110,#8111);
#7256=AXIS2_PLACEMENT_3D('',#9710,#8114,#8115);
#7257=AXIS2_PLACEMENT_3D('',#9713,#8117,#8118);
#7258=AXIS2_PLACEMENT_3D('',#9714,#8119,#8120);
#7259=AXIS2_PLACEMENT_3D('',#9718,#8123,#8124);
#7260=AXIS2_PLACEMENT_3D('',#9721,#8126,#8127);
#7261=AXIS2_PLACEMENT_3D('',#9722,#8128,#8129);
#7262=AXIS2_PLACEMENT_3D('',#9724,#8131,#8132);
#7263=AXIS2_PLACEMENT_3D('',#9730,#8136,#8137);
#7264=AXIS2_PLACEMENT_3D('',#9733,#8139,#8140);
#7265=AXIS2_PLACEMENT_3D('',#9734,#8141,#8142);
#7266=AXIS2_PLACEMENT_3D('',#9738,#8145,#8146);
#7267=AXIS2_PLACEMENT_3D('',#9741,#8148,#8149);
#7268=AXIS2_PLACEMENT_3D('',#9742,#8150,#8151);
#7269=AXIS2_PLACEMENT_3D('',#9746,#8153,#8154);
#7270=AXIS2_PLACEMENT_3D('',#9749,#8156,#8157);
#7271=AXIS2_PLACEMENT_3D('',#9750,#8158,#8159);
#7272=AXIS2_PLACEMENT_3D('',#9752,#8161,#8162);
#7273=AXIS2_PLACEMENT_3D('',#9754,#8164,#8165);
#7274=AXIS2_PLACEMENT_3D('',#9756,#8167,#8168);
#7275=AXIS2_PLACEMENT_3D('',#9757,#8169,#8170);
#7276=AXIS2_PLACEMENT_3D('',#9760,#8173,#8174);
#7277=AXIS2_PLACEMENT_3D('',#9762,#8176,#8177);
#7278=AXIS2_PLACEMENT_3D('',#9763,#8178,#8179);
#7279=AXIS2_PLACEMENT_3D('',#9764,#8180,#8181);
#7280=AXIS2_PLACEMENT_3D('',#9765,#8182,#8183);
#7281=AXIS2_PLACEMENT_3D('',#9777,#8185,#8186);
#7282=AXIS2_PLACEMENT_3D('',#9782,#8187,#8188);
#7283=AXIS2_PLACEMENT_3D('',#9827,#8190,#8191);
#7284=AXIS2_PLACEMENT_3D('',#9828,#8192,#8193);
#7285=AXIS2_PLACEMENT_3D('',#9871,#8195,#8196);
#7286=AXIS2_PLACEMENT_3D('',#9894,#8198,#8199);
#7287=AXIS2_PLACEMENT_3D('',#9914,#8200,#8201);
#7288=AXIS2_PLACEMENT_3D('',#9954,#8203,#8204);
#7289=AXIS2_PLACEMENT_3D('',#9956,#8205,#8206);
#7290=AXIS2_PLACEMENT_3D('',#9960,#8208,#8209);
#7291=AXIS2_PLACEMENT_3D('',#9961,#8210,#8211);
#7292=AXIS2_PLACEMENT_3D('',#9962,#8212,#8213);
#7293=AXIS2_PLACEMENT_3D('',#9965,#8214,#8215);
#7294=AXIS2_PLACEMENT_3D('',#9966,#8216,#8217);
#7295=AXIS2_PLACEMENT_3D('',#9969,#8220,#8221);
#7296=AXIS2_PLACEMENT_3D('',#9972,#8222,#8223);
#7297=AXIS2_PLACEMENT_3D('',#10046,#8224,#8225);
#7298=AXIS2_PLACEMENT_3D('',#10120,#8226,#8227);
#7299=AXIS2_PLACEMENT_3D('',#10194,#8228,#8229);
#7300=AXIS2_PLACEMENT_3D('',#10268,#8230,#8231);
#7301=AXIS2_PLACEMENT_3D('',#10342,#8232,#8233);
#7302=AXIS2_PLACEMENT_3D('',#10416,#8234,#8235);
#7303=AXIS2_PLACEMENT_3D('',#10490,#8236,#8237);
#7304=AXIS2_PLACEMENT_3D('',#10564,#8238,#8239);
#7305=AXIS2_PLACEMENT_3D('',#10709,#8240,#8241);
#7306=AXIS2_PLACEMENT_3D('',#10783,#8242,#8243);
#7307=AXIS2_PLACEMENT_3D('',#10857,#8244,#8245);
#7308=AXIS2_PLACEMENT_3D('',#10931,#8246,#8247);
#7309=AXIS2_PLACEMENT_3D('',#11005,#8248,#8249);
#7310=AXIS2_PLACEMENT_3D('',#11079,#8250,#8251);
#7311=AXIS2_PLACEMENT_3D('',#11153,#8252,#8253);
#7312=AXIS2_PLACEMENT_3D('',#11227,#8254,#8255);
#7313=AXIS2_PLACEMENT_3D('',#11301,#8256,#8257);
#7314=AXIS2_PLACEMENT_3D('',#11375,#8258,#8259);
#7315=AXIS2_PLACEMENT_3D('',#11447,#8260,#8261);
#7316=AXIS2_PLACEMENT_3D('',#11450,#8263,#8264);
#7317=AXIS2_PLACEMENT_3D('',#11451,#8265,#8266);
#7318=AXIS2_PLACEMENT_3D('',#11453,#8267,#8268);
#7319=AXIS2_PLACEMENT_3D('',#11454,#8269,#8270);
#7320=AXIS2_PLACEMENT_3D('',#11458,#8272,#8273);
#7321=AXIS2_PLACEMENT_3D('',#11459,#8274,#8275);
#7322=AXIS2_PLACEMENT_3D('',#11460,#8276,#8277);
#7323=AXIS2_PLACEMENT_3D('',#11464,#8280,#8281);
#7324=AXIS2_PLACEMENT_3D('',#11465,#8282,#8283);
#7325=AXIS2_PLACEMENT_3D('',#11495,#8284,#8285);
#7326=AXIS2_PLACEMENT_3D('',#11496,#8286,#8287);
#7327=AXIS2_PLACEMENT_3D('',#11526,#8288,#8289);
#7328=AXIS2_PLACEMENT_3D('',#11527,#8290,#8291);
#7329=AXIS2_PLACEMENT_3D('',#11557,#8292,#8293);
#7330=AXIS2_PLACEMENT_3D('',#11558,#8294,#8295);
#7331=AXIS2_PLACEMENT_3D('',#11588,#8296,#8297);
#7332=AXIS2_PLACEMENT_3D('',#11589,#8298,#8299);
#7333=AXIS2_PLACEMENT_3D('',#11619,#8300,#8301);
#7334=AXIS2_PLACEMENT_3D('',#11620,#8302,#8303);
#7335=AXIS2_PLACEMENT_3D('',#11650,#8304,#8305);
#7336=AXIS2_PLACEMENT_3D('',#11651,#8306,#8307);
#7337=AXIS2_PLACEMENT_3D('',#11681,#8308,#8309);
#7338=AXIS2_PLACEMENT_3D('',#11682,#8310,#8311);
#7339=AXIS2_PLACEMENT_3D('',#11712,#8312,#8313);
#7340=AXIS2_PLACEMENT_3D('',#11713,#8314,#8315);
#7341=AXIS2_PLACEMENT_3D('',#11743,#8316,#8317);
#7342=AXIS2_PLACEMENT_3D('',#11744,#8318,#8319);
#7343=AXIS2_PLACEMENT_3D('',#11774,#8320,#8321);
#7344=AXIS2_PLACEMENT_3D('',#11775,#8322,#8323);
#7345=AXIS2_PLACEMENT_3D('',#11805,#8324,#8325);
#7346=AXIS2_PLACEMENT_3D('',#11806,#8326,#8327);
#7347=AXIS2_PLACEMENT_3D('',#11836,#8328,#8329);
#7348=AXIS2_PLACEMENT_3D('',#11837,#8330,#8331);
#7349=AXIS2_PLACEMENT_3D('',#11867,#8332,#8333);
#7350=AXIS2_PLACEMENT_3D('',#11868,#8334,#8335);
#7351=AXIS2_PLACEMENT_3D('',#11898,#8336,#8337);
#7352=AXIS2_PLACEMENT_3D('',#11899,#8338,#8339);
#7353=AXIS2_PLACEMENT_3D('',#11929,#8340,#8341);
#7354=AXIS2_PLACEMENT_3D('',#11930,#8342,#8343);
#7355=AXIS2_PLACEMENT_3D('',#11960,#8344,#8345);
#7356=AXIS2_PLACEMENT_3D('',#11961,#8346,#8347);
#7357=AXIS2_PLACEMENT_3D('',#11991,#8348,#8349);
#7358=AXIS2_PLACEMENT_3D('',#11992,#8350,#8351);
#7359=AXIS2_PLACEMENT_3D('',#12022,#8352,#8353);
#7360=AXIS2_PLACEMENT_3D('',#12023,#8354,#8355);
#7361=AXIS2_PLACEMENT_3D('',#12053,#8356,#8357);
#7362=AXIS2_PLACEMENT_3D('',#12054,#8358,#8359);
#7363=AXIS2_PLACEMENT_3D('',#12056,#8360,#8361);
#7364=AXIS2_PLACEMENT_3D('',#12059,#8363,#8364);
#7365=AXIS2_PLACEMENT_3D('',#12060,#8365,#8366);
#7366=AXIS2_PLACEMENT_3D('',#12063,#8368,#8369);
#7367=AXIS2_PLACEMENT_3D('',#12064,#8370,#8371);
#7368=AXIS2_PLACEMENT_3D('',#12094,#8372,#8373);
#7369=AXIS2_PLACEMENT_3D('',#13428,#8394,#8395);
#7370=AXIS2_PLACEMENT_3D('',#13429,#8396,#8397);
#7371=AXIS2_PLACEMENT_3D('',#13430,#8398,#8399);
#7372=AXIS2_PLACEMENT_3D('',#13433,#8401,#8402);
#7373=AXIS2_PLACEMENT_3D('',#13441,#8403,#8404);
#7374=AXIS2_PLACEMENT_3D('',#13471,#8405,#8406);
#7375=AXIS2_PLACEMENT_3D('',#13513,#8407,#8408);
#7376=AXIS2_PLACEMENT_3D('',#13555,#8409,#8410);
#7377=AXIS2_PLACEMENT_3D('',#13597,#8411,#8412);
#7378=AXIS2_PLACEMENT_3D('',#13627,#8413,#8414);
#7379=AXIS2_PLACEMENT_3D('',#13657,#8415,#8416);
#7380=AXIS2_PLACEMENT_3D('',#13699,#8417,#8418);
#7381=AXIS2_PLACEMENT_3D('',#13741,#8419,#8420);
#7382=AXIS2_PLACEMENT_3D('',#13771,#8421,#8422);
#7383=AXIS2_PLACEMENT_3D('',#13801,#8423,#8424);
#7384=AXIS2_PLACEMENT_3D('',#13843,#8425,#8426);
#7385=AXIS2_PLACEMENT_3D('',#13885,#8427,#8428);
#7386=AXIS2_PLACEMENT_3D('',#13927,#8429,#8430);
#7387=AXIS2_PLACEMENT_3D('',#13957,#8431,#8432);
#7388=AXIS2_PLACEMENT_3D('',#13987,#8433,#8434);
#7389=AXIS2_PLACEMENT_3D('',#14029,#8435,#8436);
#7390=AXIS2_PLACEMENT_3D('',#14071,#8437,#8438);
#7391=AXIS2_PLACEMENT_3D('',#14113,#8439,#8440);
#7392=AXIS2_PLACEMENT_3D('',#14230,#8441,#8442);
#7393=AXIS2_PLACEMENT_3D('',#14347,#8443,#8444);
#7394=AXIS2_PLACEMENT_3D('',#14402,#8445,#8446);
#7395=AXIS2_PLACEMENT_3D('',#14457,#8447,#8448);
#7396=AXIS2_PLACEMENT_3D('',#14574,#8449,#8450);
#7397=AXIS2_PLACEMENT_3D('',#14691,#8451,#8452);
#7398=AXIS2_PLACEMENT_3D('',#14808,#8453,#8454);
#7399=AXIS2_PLACEMENT_3D('',#14863,#8455,#8456);
#7400=AXIS2_PLACEMENT_3D('',#14918,#8457,#8458);
#7401=AXIS2_PLACEMENT_3D('',#15035,#8459,#8460);
#7402=AXIS2_PLACEMENT_3D('',#15152,#8461,#8462);
#7403=AXIS2_PLACEMENT_3D('',#15269,#8463,#8464);
#7404=AXIS2_PLACEMENT_3D('',#15324,#8465,#8466);
#7405=AXIS2_PLACEMENT_3D('',#15379,#8467,#8468);
#7406=AXIS2_PLACEMENT_3D('',#15496,#8469,#8470);
#7407=AXIS2_PLACEMENT_3D('',#15613,#8471,#8472);
#7408=AXIS2_PLACEMENT_3D('',#15730,#8473,#8474);
#7409=AXIS2_PLACEMENT_3D('',#15785,#8475,#8476);
#7410=AXIS2_PLACEMENT_3D('',#15840,#8477,#8478);
#7411=AXIS2_PLACEMENT_3D('',#15841,#8479,#8480);
#7412=AXIS2_PLACEMENT_3D('',#15842,#8481,#8482);
#7413=AXIS2_PLACEMENT_3D('',#15843,#8483,#8484);
#7414=AXIS2_PLACEMENT_3D('',#15888,#8486,#8487);
#7415=AXIS2_PLACEMENT_3D('',#15889,#8488,#8489);
#7416=AXIS2_PLACEMENT_3D('',#15932,#8491,#8492);
#7417=AXIS2_PLACEMENT_3D('',#15955,#8494,#8495);
#7418=AXIS2_PLACEMENT_3D('',#15975,#8496,#8497);
#7419=AXIS2_PLACEMENT_3D('',#16015,#8499,#8500);
#7420=AXIS2_PLACEMENT_3D('',#16017,#8501,#8502);
#7421=AXIS2_PLACEMENT_3D('',#16021,#8504,#8505);
#7422=AXIS2_PLACEMENT_3D('',#16022,#8506,#8507);
#7423=AXIS2_PLACEMENT_3D('',#16023,#8508,#8509);
#7424=AXIS2_PLACEMENT_3D('',#16026,#8510,#8511);
#7425=AXIS2_PLACEMENT_3D('',#16027,#8512,#8513);
#7426=AXIS2_PLACEMENT_3D('',#16030,#8516,#8517);
#7427=AXIS2_PLACEMENT_3D('',#16033,#8518,#8519);
#7428=AXIS2_PLACEMENT_3D('',#16107,#8520,#8521);
#7429=AXIS2_PLACEMENT_3D('',#16181,#8522,#8523);
#7430=AXIS2_PLACEMENT_3D('',#16255,#8524,#8525);
#7431=AXIS2_PLACEMENT_3D('',#16329,#8526,#8527);
#7432=AXIS2_PLACEMENT_3D('',#16403,#8528,#8529);
#7433=AXIS2_PLACEMENT_3D('',#16477,#8530,#8531);
#7434=AXIS2_PLACEMENT_3D('',#16551,#8532,#8533);
#7435=AXIS2_PLACEMENT_3D('',#16625,#8534,#8535);
#7436=AXIS2_PLACEMENT_3D('',#16699,#8536,#8537);
#7437=AXIS2_PLACEMENT_3D('',#16773,#8538,#8539);
#7438=AXIS2_PLACEMENT_3D('',#16847,#8540,#8541);
#7439=AXIS2_PLACEMENT_3D('',#16921,#8542,#8543);
#7440=AXIS2_PLACEMENT_3D('',#16995,#8544,#8545);
#7441=AXIS2_PLACEMENT_3D('',#17069,#8546,#8547);
#7442=AXIS2_PLACEMENT_3D('',#17143,#8548,#8549);
#7443=AXIS2_PLACEMENT_3D('',#17217,#8550,#8551);
#7444=AXIS2_PLACEMENT_3D('',#17291,#8552,#8553);
#7445=AXIS2_PLACEMENT_3D('',#17365,#8554,#8555);
#7446=AXIS2_PLACEMENT_3D('',#17439,#8556,#8557);
#7447=AXIS2_PLACEMENT_3D('',#17511,#8558,#8559);
#7448=AXIS2_PLACEMENT_3D('',#17514,#8561,#8562);
#7449=AXIS2_PLACEMENT_3D('',#17515,#8563,#8564);
#7450=AXIS2_PLACEMENT_3D('',#17517,#8565,#8566);
#7451=AXIS2_PLACEMENT_3D('',#17518,#8567,#8568);
#7452=AXIS2_PLACEMENT_3D('',#17522,#8570,#8571);
#7453=AXIS2_PLACEMENT_3D('',#17523,#8572,#8573);
#7454=AXIS2_PLACEMENT_3D('',#17524,#8574,#8575);
#7455=AXIS2_PLACEMENT_3D('',#17528,#8578,#8579);
#7456=AXIS2_PLACEMENT_3D('',#17529,#8580,#8581);
#7457=AXIS2_PLACEMENT_3D('',#17557,#8582,#8583);
#7458=AXIS2_PLACEMENT_3D('',#17558,#8584,#8585);
#7459=AXIS2_PLACEMENT_3D('',#17586,#8586,#8587);
#7460=AXIS2_PLACEMENT_3D('',#17587,#8588,#8589);
#7461=AXIS2_PLACEMENT_3D('',#17615,#8590,#8591);
#7462=AXIS2_PLACEMENT_3D('',#17616,#8592,#8593);
#7463=AXIS2_PLACEMENT_3D('',#17644,#8594,#8595);
#7464=AXIS2_PLACEMENT_3D('',#17645,#8596,#8597);
#7465=AXIS2_PLACEMENT_3D('',#17673,#8598,#8599);
#7466=AXIS2_PLACEMENT_3D('',#17674,#8600,#8601);
#7467=AXIS2_PLACEMENT_3D('',#17702,#8602,#8603);
#7468=AXIS2_PLACEMENT_3D('',#17703,#8604,#8605);
#7469=AXIS2_PLACEMENT_3D('',#17731,#8606,#8607);
#7470=AXIS2_PLACEMENT_3D('',#17732,#8608,#8609);
#7471=AXIS2_PLACEMENT_3D('',#17760,#8610,#8611);
#7472=AXIS2_PLACEMENT_3D('',#17761,#8612,#8613);
#7473=AXIS2_PLACEMENT_3D('',#17789,#8614,#8615);
#7474=AXIS2_PLACEMENT_3D('',#17790,#8616,#8617);
#7475=AXIS2_PLACEMENT_3D('',#17818,#8618,#8619);
#7476=AXIS2_PLACEMENT_3D('',#17819,#8620,#8621);
#7477=AXIS2_PLACEMENT_3D('',#17847,#8622,#8623);
#7478=AXIS2_PLACEMENT_3D('',#17848,#8624,#8625);
#7479=AXIS2_PLACEMENT_3D('',#17876,#8626,#8627);
#7480=AXIS2_PLACEMENT_3D('',#17877,#8628,#8629);
#7481=AXIS2_PLACEMENT_3D('',#17905,#8630,#8631);
#7482=AXIS2_PLACEMENT_3D('',#17906,#8632,#8633);
#7483=AXIS2_PLACEMENT_3D('',#17934,#8634,#8635);
#7484=AXIS2_PLACEMENT_3D('',#17935,#8636,#8637);
#7485=AXIS2_PLACEMENT_3D('',#17963,#8638,#8639);
#7486=AXIS2_PLACEMENT_3D('',#17964,#8640,#8641);
#7487=AXIS2_PLACEMENT_3D('',#17992,#8642,#8643);
#7488=AXIS2_PLACEMENT_3D('',#17993,#8644,#8645);
#7489=AXIS2_PLACEMENT_3D('',#18021,#8646,#8647);
#7490=AXIS2_PLACEMENT_3D('',#18022,#8648,#8649);
#7491=AXIS2_PLACEMENT_3D('',#18050,#8650,#8651);
#7492=AXIS2_PLACEMENT_3D('',#18051,#8652,#8653);
#7493=AXIS2_PLACEMENT_3D('',#18079,#8654,#8655);
#7494=AXIS2_PLACEMENT_3D('',#18080,#8656,#8657);
#7495=AXIS2_PLACEMENT_3D('',#18082,#8658,#8659);
#7496=AXIS2_PLACEMENT_3D('',#18085,#8661,#8662);
#7497=AXIS2_PLACEMENT_3D('',#18086,#8663,#8664);
#7498=AXIS2_PLACEMENT_3D('',#18089,#8666,#8667);
#7499=AXIS2_PLACEMENT_3D('',#18090,#8668,#8669);
#7500=AXIS2_PLACEMENT_3D('',#18118,#8670,#8671);
#7501=AXIS2_PLACEMENT_3D('',#19398,#8692,#8693);
#7502=AXIS2_PLACEMENT_3D('',#19399,#8694,#8695);
#7503=AXIS2_PLACEMENT_3D('',#19400,#8696,#8697);
#7504=AXIS2_PLACEMENT_3D('',#19403,#8699,#8700);
#7505=AXIS2_PLACEMENT_3D('',#19433,#8701,#8702);
#7506=AXIS2_PLACEMENT_3D('',#19463,#8703,#8704);
#7507=AXIS2_PLACEMENT_3D('',#19493,#8705,#8706);
#7508=AXIS2_PLACEMENT_3D('',#19523,#8707,#8708);
#7509=AXIS2_PLACEMENT_3D('',#19553,#8709,#8710);
#7510=AXIS2_PLACEMENT_3D('',#19583,#8711,#8712);
#7511=AXIS2_PLACEMENT_3D('',#19613,#8713,#8714);
#7512=AXIS2_PLACEMENT_3D('',#19643,#8715,#8716);
#7513=AXIS2_PLACEMENT_3D('',#19673,#8717,#8718);
#7514=AXIS2_PLACEMENT_3D('',#19703,#8719,#8720);
#7515=AXIS2_PLACEMENT_3D('',#19733,#8721,#8722);
#7516=AXIS2_PLACEMENT_3D('',#19763,#8723,#8724);
#7517=AXIS2_PLACEMENT_3D('',#19793,#8725,#8726);
#7518=AXIS2_PLACEMENT_3D('',#19823,#8727,#8728);
#7519=AXIS2_PLACEMENT_3D('',#19853,#8729,#8730);
#7520=AXIS2_PLACEMENT_3D('',#19883,#8731,#8732);
#7521=AXIS2_PLACEMENT_3D('',#19913,#8733,#8734);
#7522=AXIS2_PLACEMENT_3D('',#19943,#8735,#8736);
#7523=AXIS2_PLACEMENT_3D('',#19973,#8737,#8738);
#7524=AXIS2_PLACEMENT_3D('',#20024,#8739,#8740);
#7525=AXIS2_PLACEMENT_3D('',#20079,#8741,#8742);
#7526=AXIS2_PLACEMENT_3D('',#20134,#8743,#8744);
#7527=AXIS2_PLACEMENT_3D('',#20185,#8745,#8746);
#7528=AXIS2_PLACEMENT_3D('',#20236,#8747,#8748);
#7529=AXIS2_PLACEMENT_3D('',#20287,#8749,#8750);
#7530=AXIS2_PLACEMENT_3D('',#20342,#8751,#8752);
#7531=AXIS2_PLACEMENT_3D('',#20397,#8753,#8754);
#7532=AXIS2_PLACEMENT_3D('',#20448,#8755,#8756);
#7533=AXIS2_PLACEMENT_3D('',#20499,#8757,#8758);
#7534=AXIS2_PLACEMENT_3D('',#20550,#8759,#8760);
#7535=AXIS2_PLACEMENT_3D('',#20605,#8761,#8762);
#7536=AXIS2_PLACEMENT_3D('',#20660,#8763,#8764);
#7537=AXIS2_PLACEMENT_3D('',#20711,#8765,#8766);
#7538=AXIS2_PLACEMENT_3D('',#20762,#8767,#8768);
#7539=AXIS2_PLACEMENT_3D('',#20813,#8769,#8770);
#7540=AXIS2_PLACEMENT_3D('',#20868,#8771,#8772);
#7541=AXIS2_PLACEMENT_3D('',#20923,#8773,#8774);
#7542=AXIS2_PLACEMENT_3D('',#20974,#8775,#8776);
#7543=AXIS2_PLACEMENT_3D('',#20975,#8777,#8778);
#7544=AXIS2_PLACEMENT_3D('',#20976,#8779,#8780);
#7545=AXIS2_PLACEMENT_3D('',#20977,#8781,#8782);
#7546=AXIS2_PLACEMENT_3D('',#20980,#8783,#8784);
#7547=AXIS2_PLACEMENT_3D('',#20983,#8786,#8787);
#7548=AXIS2_PLACEMENT_3D('',#20984,#8788,#8789);
#7549=AXIS2_PLACEMENT_3D('',#20987,#8790,#8791);
#7550=AXIS2_PLACEMENT_3D('',#20990,#8793,#8794);
#7551=AXIS2_PLACEMENT_3D('',#20991,#8795,#8796);
#7552=AXIS2_PLACEMENT_3D('',#20994,#8799,#8800);
#7553=AXIS2_PLACEMENT_3D('',#20997,#8801,#8802);
#7554=AXIS2_PLACEMENT_3D('',#20999,#8804,#8805);
#7555=AXIS2_PLACEMENT_3D('',#21005,#8809,#8810);
#7556=AXIS2_PLACEMENT_3D('',#21006,#8811,#8812);
#7557=AXIS2_PLACEMENT_3D('',#21007,#8813,#8814);
#7558=AXIS2_PLACEMENT_3D('',#21011,#8816,#8817);
#7559=AXIS2_PLACEMENT_3D('',#21012,#8818,#8819);
#7560=AXIS2_PLACEMENT_3D('',#21015,#8821,#8822);
#7561=AXIS2_PLACEMENT_3D('',#21016,#8823,#8824);
#7562=AXIS2_PLACEMENT_3D('',#21018,#8825,#8826);
#7563=AXIS2_PLACEMENT_3D('',#21021,#8828,#8829);
#7564=AXIS2_PLACEMENT_3D('',#21022,#8830,#8831);
#7565=AXIS2_PLACEMENT_3D('',#21025,#8833,#8834);
#7566=AXIS2_PLACEMENT_3D('',#21027,#8835,#8836);
#7567=AXIS2_PLACEMENT_3D('',#21028,#8837,#8838);
#7568=AXIS2_PLACEMENT_3D('',#21030,#8839,#8840);
#7569=AXIS2_PLACEMENT_3D('',#21032,#8842,#8843);
#7570=AXIS2_PLACEMENT_3D('',#21034,#8844,#8845);
#7571=AXIS2_PLACEMENT_3D('',#21037,#8848,#8849);
#7572=AXIS2_PLACEMENT_3D('',#21039,#8850,#8851);
#7573=AXIS2_PLACEMENT_3D('',#21041,#8853,#8854);
#7574=AXIS2_PLACEMENT_3D('',#21042,#8855,#8856);
#7575=AXIS2_PLACEMENT_3D('',#21043,#8857,#8858);
#7576=AXIS2_PLACEMENT_3D('',#21046,#8859,#8860);
#7577=AXIS2_PLACEMENT_3D('',#21049,#8862,#8863);
#7578=AXIS2_PLACEMENT_3D('',#21050,#8864,#8865);
#7579=AXIS2_PLACEMENT_3D('',#21053,#8866,#8867);
#7580=AXIS2_PLACEMENT_3D('',#21056,#8869,#8870);
#7581=AXIS2_PLACEMENT_3D('',#21057,#8871,#8872);
#7582=AXIS2_PLACEMENT_3D('',#21060,#8875,#8876);
#7583=AXIS2_PLACEMENT_3D('',#21063,#8877,#8878);
#7584=AXIS2_PLACEMENT_3D('',#21065,#8880,#8881);
#7585=AXIS2_PLACEMENT_3D('',#21071,#8885,#8886);
#7586=AXIS2_PLACEMENT_3D('',#21072,#8887,#8888);
#7587=AXIS2_PLACEMENT_3D('',#21073,#8889,#8890);
#7588=AXIS2_PLACEMENT_3D('',#21077,#8892,#8893);
#7589=AXIS2_PLACEMENT_3D('',#21078,#8894,#8895);
#7590=AXIS2_PLACEMENT_3D('',#21081,#8897,#8898);
#7591=AXIS2_PLACEMENT_3D('',#21082,#8899,#8900);
#7592=AXIS2_PLACEMENT_3D('',#21084,#8901,#8902);
#7593=AXIS2_PLACEMENT_3D('',#21087,#8904,#8905);
#7594=AXIS2_PLACEMENT_3D('',#21088,#8906,#8907);
#7595=AXIS2_PLACEMENT_3D('',#21091,#8909,#8910);
#7596=AXIS2_PLACEMENT_3D('',#21093,#8911,#8912);
#7597=AXIS2_PLACEMENT_3D('',#21094,#8913,#8914);
#7598=AXIS2_PLACEMENT_3D('',#21096,#8915,#8916);
#7599=AXIS2_PLACEMENT_3D('',#21098,#8918,#8919);
#7600=AXIS2_PLACEMENT_3D('',#21100,#8920,#8921);
#7601=AXIS2_PLACEMENT_3D('',#21103,#8924,#8925);
#7602=AXIS2_PLACEMENT_3D('',#21105,#8926,#8927);
#7603=AXIS2_PLACEMENT_3D('',#21107,#8929,#8930);
#7604=AXIS2_PLACEMENT_3D('',#21108,#8931,#8932);
#7605=AXIS2_PLACEMENT_3D('',#21109,#8933,#8934);
#7606=AXIS2_PLACEMENT_3D('',#21112,#8935,#8936);
#7607=AXIS2_PLACEMENT_3D('',#21187,#8937,#8938);
#7608=AXIS2_PLACEMENT_3D('',#21189,#8939,#8940);
#7609=AXIS2_PLACEMENT_3D('',#21198,#8942,#8943);
#7610=AXIS2_PLACEMENT_3D('',#21207,#8944,#8945);
#7611=AXIS2_PLACEMENT_3D('',#21216,#8946,#8947);
#7612=AXIS2_PLACEMENT_3D('',#21225,#8948,#8949);
#7613=AXIS2_PLACEMENT_3D('',#21234,#8950,#8951);
#7614=AXIS2_PLACEMENT_3D('',#21242,#8952,#8953);
#7615=AXIS2_PLACEMENT_3D('',#21244,#8954,#8955);
#7616=AXIS2_PLACEMENT_3D('',#21253,#8956,#8957);
#7617=AXIS2_PLACEMENT_3D('',#21262,#8958,#8959);
#7618=AXIS2_PLACEMENT_3D('',#21271,#8960,#8961);
#7619=AXIS2_PLACEMENT_3D('',#21276,#8962,#8963);
#7620=AXIS2_PLACEMENT_3D('',#21278,#8964,#8965);
#7621=AXIS2_PLACEMENT_3D('',#21290,#8966,#8967);
#7622=AXIS2_PLACEMENT_3D('',#21292,#8968,#8969);
#7623=AXIS2_PLACEMENT_3D('',#21301,#8970,#8971);
#7624=AXIS2_PLACEMENT_3D('',#21310,#8972,#8973);
#7625=AXIS2_PLACEMENT_3D('',#21319,#8974,#8975);
#7626=AXIS2_PLACEMENT_3D('',#21327,#8977,#8978);
#7627=AXIS2_PLACEMENT_3D('',#21334,#8979,#8980);
#7628=AXIS2_PLACEMENT_3D('',#21343,#8981,#8982);
#7629=AXIS2_PLACEMENT_3D('',#21352,#8983,#8984);
#7630=AXIS2_PLACEMENT_3D('',#21361,#8985,#8986);
#7631=AXIS2_PLACEMENT_3D('',#21370,#8987,#8988);
#7632=AXIS2_PLACEMENT_3D('',#21378,#8989,#8990);
#7633=AXIS2_PLACEMENT_3D('',#21379,#8991,#8992);
#7634=AXIS2_PLACEMENT_3D('',#21381,#8993,#8994);
#7635=AXIS2_PLACEMENT_3D('',#21392,#8995,#8996);
#7636=AXIS2_PLACEMENT_3D('',#21395,#8997,#8998);
#7637=AXIS2_PLACEMENT_3D('',#21431,#8999,#9000);
#7638=AXIS2_PLACEMENT_3D('',#21433,#9001,#9002);
#7639=AXIS2_PLACEMENT_3D('',#21445,#9003,#9004);
#7640=AXIS2_PLACEMENT_3D('',#21447,#9005,#9006);
#7641=AXIS2_PLACEMENT_3D('',#21458,#9007,#9008);
#7642=AXIS2_PLACEMENT_3D('',#21461,#9009,#9010);
#7643=AXIS2_PLACEMENT_3D('',#21497,#9011,#9012);
#7644=AXIS2_PLACEMENT_3D('',#21499,#9013,#9014);
#7645=AXIS2_PLACEMENT_3D('',#21511,#9015,#9016);
#7646=AXIS2_PLACEMENT_3D('',#21513,#9017,#9018);
#7647=AXIS2_PLACEMENT_3D('',#21524,#9019,#9020);
#7648=AXIS2_PLACEMENT_3D('',#21527,#9021,#9022);
#7649=AXIS2_PLACEMENT_3D('',#21563,#9023,#9024);
#7650=AXIS2_PLACEMENT_3D('',#21565,#9025,#9026);
#7651=AXIS2_PLACEMENT_3D('',#21577,#9027,#9028);
#7652=AXIS2_PLACEMENT_3D('',#21579,#9029,#9030);
#7653=AXIS2_PLACEMENT_3D('',#21590,#9031,#9032);
#7654=AXIS2_PLACEMENT_3D('',#21593,#9033,#9034);
#7655=AXIS2_PLACEMENT_3D('',#21635,#9035,#9036);
#7656=AXIS2_PLACEMENT_3D('',#21637,#9037,#9038);
#7657=AXIS2_PLACEMENT_3D('',#21649,#9039,#9040);
#7658=AXIS2_PLACEMENT_3D('',#21651,#9041,#9042);
#7659=AXIS2_PLACEMENT_3D('',#21662,#9043,#9044);
#7660=AXIS2_PLACEMENT_3D('',#21665,#9045,#9046);
#7661=AXIS2_PLACEMENT_3D('',#21701,#9047,#9048);
#7662=AXIS2_PLACEMENT_3D('',#21703,#9049,#9050);
#7663=AXIS2_PLACEMENT_3D('',#21715,#9051,#9052);
#7664=AXIS2_PLACEMENT_3D('',#21717,#9053,#9054);
#7665=AXIS2_PLACEMENT_3D('',#21728,#9055,#9056);
#7666=AXIS2_PLACEMENT_3D('',#21731,#9057,#9058);
#7667=AXIS2_PLACEMENT_3D('',#21767,#9059,#9060);
#7668=AXIS2_PLACEMENT_3D('',#21769,#9061,#9062);
#7669=AXIS2_PLACEMENT_3D('',#21781,#9063,#9064);
#7670=AXIS2_PLACEMENT_3D('',#21783,#9065,#9066);
#7671=AXIS2_PLACEMENT_3D('',#21794,#9067,#9068);
#7672=AXIS2_PLACEMENT_3D('',#21797,#9069,#9070);
#7673=AXIS2_PLACEMENT_3D('',#21833,#9071,#9072);
#7674=AXIS2_PLACEMENT_3D('',#21835,#9073,#9074);
#7675=AXIS2_PLACEMENT_3D('',#21847,#9075,#9076);
#7676=AXIS2_PLACEMENT_3D('',#21849,#9077,#9078);
#7677=AXIS2_PLACEMENT_3D('',#21860,#9079,#9080);
#7678=AXIS2_PLACEMENT_3D('',#21863,#9081,#9082);
#7679=AXIS2_PLACEMENT_3D('',#21899,#9083,#9084);
#7680=AXIS2_PLACEMENT_3D('',#21901,#9085,#9086);
#7681=AXIS2_PLACEMENT_3D('',#21909,#9087,#9088);
#7682=AXIS2_PLACEMENT_3D('',#21912,#9090,#9091);
#7683=AXIS2_PLACEMENT_3D('',#21913,#9092,#9093);
#7684=AXIS2_PLACEMENT_3D('',#21925,#9094,#9095);
#7685=AXIS2_PLACEMENT_3D('',#21927,#9096,#9097);
#7686=AXIS2_PLACEMENT_3D('',#21930,#9099,#9100);
#7687=AXIS2_PLACEMENT_3D('',#21938,#9101,#9102);
#7688=AXIS2_PLACEMENT_3D('',#21939,#9103,#9104);
#7689=AXIS2_PLACEMENT_3D('',#21950,#9105,#9106);
#7690=AXIS2_PLACEMENT_3D('',#21953,#9107,#9108);
#7691=AXIS2_PLACEMENT_3D('',#21975,#9109,#9110);
#7692=AXIS2_PLACEMENT_3D('',#21976,#9111,#9112);
#7693=AXIS2_PLACEMENT_3D('',#21978,#9113,#9114);
#7694=AXIS2_PLACEMENT_3D('',#21979,#9115,#9116);
#7695=AXIS2_PLACEMENT_3D('',#21981,#9117,#9118);
#7696=AXIS2_PLACEMENT_3D('',#21983,#9120,#9121);
#7697=AXIS2_PLACEMENT_3D('',#21985,#9122,#9123);
#7698=AXIS2_PLACEMENT_3D('',#21987,#9125,#9126);
#7699=AXIS2_PLACEMENT_3D('',#21989,#9127,#9128);
#7700=AXIS2_PLACEMENT_3D('',#21991,#9130,#9131);
#7701=AXIS2_PLACEMENT_3D('',#21993,#9132,#9133);
#7702=AXIS2_PLACEMENT_3D('',#21994,#9134,#9135);
#7703=AXIS2_PLACEMENT_3D('',#21996,#9137,#9138);
#7704=AXIS2_PLACEMENT_3D('',#21997,#9139,#9140);
#7705=AXIS2_PLACEMENT_3D('',#21999,#9141,#9142);
#7706=AXIS2_PLACEMENT_3D('',#22000,#9143,#9144);
#7707=AXIS2_PLACEMENT_3D('',#22003,#9146,#9147);
#7708=AXIS2_PLACEMENT_3D('',#22004,#9148,#9149);
#7709=AXIS2_PLACEMENT_3D('',#22007,#9151,#9152);
#7710=AXIS2_PLACEMENT_3D('',#22008,#9153,#9154);
#7711=AXIS2_PLACEMENT_3D('',#22011,#9156,#9157);
#7712=AXIS2_PLACEMENT_3D('',#22012,#9158,#9159);
#7713=AXIS2_PLACEMENT_3D('',#22013,#9160,#9161);
#7714=AXIS2_PLACEMENT_3D('',#22014,#9162,#9163);
#7715=AXIS2_PLACEMENT_3D('',#22016,#9164,#9165);
#7716=AXIS2_PLACEMENT_3D('',#22018,#9166,#9167);
#7717=AXIS2_PLACEMENT_3D('',#22019,#9168,#9169);
#7718=AXIS2_PLACEMENT_3D('',#22021,#9170,#9171);
#7719=AXIS2_PLACEMENT_3D('',#22023,#9173,#9174);
#7720=AXIS2_PLACEMENT_3D('',#22025,#9175,#9176);
#7721=AXIS2_PLACEMENT_3D('',#22026,#9177,#9178);
#7722=AXIS2_PLACEMENT_3D('',#22029,#9180,#9181);
#7723=AXIS2_PLACEMENT_3D('',#22030,#9182,#9183);
#7724=AXIS2_PLACEMENT_3D('',#22032,#9184,#9185);
#7725=AXIS2_PLACEMENT_3D('',#22033,#9186,#9187);
#7726=AXIS2_PLACEMENT_3D('',#22035,#9188,#9189);
#7727=AXIS2_PLACEMENT_3D('',#22037,#9191,#9192);
#7728=AXIS2_PLACEMENT_3D('',#22039,#9193,#9194);
#7729=AXIS2_PLACEMENT_3D('',#22041,#9196,#9197);
#7730=AXIS2_PLACEMENT_3D('',#22043,#9198,#9199);
#7731=AXIS2_PLACEMENT_3D('',#22045,#9201,#9202);
#7732=AXIS2_PLACEMENT_3D('',#22047,#9203,#9204);
#7733=AXIS2_PLACEMENT_3D('',#22048,#9205,#9206);
#7734=AXIS2_PLACEMENT_3D('',#22051,#9208,#9209);
#7735=AXIS2_PLACEMENT_3D('',#22052,#9210,#9211);
#7736=AXIS2_PLACEMENT_3D('',#22054,#9212,#9213);
#7737=AXIS2_PLACEMENT_3D('',#22055,#9214,#9215);
#7738=AXIS2_PLACEMENT_3D('',#22057,#9216,#9217);
#7739=AXIS2_PLACEMENT_3D('',#22059,#9219,#9220);
#7740=AXIS2_PLACEMENT_3D('',#22061,#9221,#9222);
#7741=AXIS2_PLACEMENT_3D('',#22062,#9223,#9224);
#7742=AXIS2_PLACEMENT_3D('',#22065,#9226,#9227);
#7743=AXIS2_PLACEMENT_3D('',#22066,#9228,#9229);
#7744=AXIS2_PLACEMENT_3D('',#22069,#9231,#9232);
#7745=AXIS2_PLACEMENT_3D('',#22070,#9233,#9234);
#7746=AXIS2_PLACEMENT_3D('',#22072,#9236,#9237);
#7747=AXIS2_PLACEMENT_3D('',#22073,#9238,#9239);
#7748=AXIS2_PLACEMENT_3D('',#22075,#9240,#9241);
#7749=AXIS2_PLACEMENT_3D('',#22078,#9243,#9244);
#7750=AXIS2_PLACEMENT_3D('',#22079,#9245,#9246);
#7751=AXIS2_PLACEMENT_3D('',#22081,#9247,#9248);
#7752=AXIS2_PLACEMENT_3D('',#22082,#9249,#9250);
#7753=AXIS2_PLACEMENT_3D('',#22085,#9252,#9253);
#7754=AXIS2_PLACEMENT_3D('',#22086,#9254,#9255);
#7755=AXIS2_PLACEMENT_3D('',#22087,#9256,#9257);
#7756=AXIS2_PLACEMENT_3D('',#22088,#9258,#9259);
#7757=AXIS2_PLACEMENT_3D('',#22104,#9261,#9262);
#7758=AXIS2_PLACEMENT_3D('',#22112,#9263,#9264);
#7759=AXIS2_PLACEMENT_3D('',#22160,#9266,#9267);
#7760=AXIS2_PLACEMENT_3D('',#22214,#9269,#9270);
#7761=AXIS2_PLACEMENT_3D('',#22262,#9272,#9273);
#7762=AXIS2_PLACEMENT_3D('',#22313,#9275,#9276);
#7763=AXIS2_PLACEMENT_3D('',#22329,#9278,#9279);
#7764=AXIS2_PLACEMENT_3D('',#22339,#9280,#9281);
#7765=AXIS2_PLACEMENT_3D('',#22363,#9283,#9284);
#7766=AXIS2_PLACEMENT_3D('',#22388,#9286,#9287);
#7767=AXIS2_PLACEMENT_3D('',#22413,#9289,#9290);
#7768=AXIS2_PLACEMENT_3D('',#22501,#9291,#9292);
#7769=AXIS2_PLACEMENT_3D('',#22503,#9293,#9294);
#7770=AXIS2_PLACEMENT_3D('',#22843,#9295,#9296);
#7771=AXIS2_PLACEMENT_3D('',#22845,#9297,#9298);
#7772=AXIS2_PLACEMENT_3D('',#22846,#9299,#9300);
#7773=AXIS2_PLACEMENT_3D('',#22939,#9301,#9302);
#7774=AXIS2_PLACEMENT_3D('',#22940,#9303,#9304);
#7775=AXIS2_PLACEMENT_3D('',#23096,#9305,#9306);
#7776=AXIS2_PLACEMENT_3D('',#23100,#9308,#9309);
#7777=AXIS2_PLACEMENT_3D('',#23101,#9310,#9311);
#7778=AXIS2_PLACEMENT_3D('',#23110,#9316,#9317);
#7779=AXIS2_PLACEMENT_3D('',#23116,#9321,#9322);
#7780=AXIS2_PLACEMENT_3D('',#23122,#9326,#9327);
#7781=AXIS2_PLACEMENT_3D('',#23128,#9331,#9332);
#7782=AXIS2_PLACEMENT_3D('',#23134,#9336,#9337);
#7783=AXIS2_PLACEMENT_3D('',#23137,#9340,#9341);
#7784=AXIS2_PLACEMENT_3D('',#23138,#9342,#9343);
#7785=AXIS2_PLACEMENT_3D('',#23140,#9344,#9345);
#7786=AXIS2_PLACEMENT_3D('',#23141,#9346,#9347);
#7787=AXIS2_PLACEMENT_3D('',#23143,#9349,#9350);
#7788=AXIS2_PLACEMENT_3D('',#23144,#9351,#9352);
#7789=AXIS2_PLACEMENT_3D('',#23145,#9353,#9354);
#7790=AXIS2_PLACEMENT_3D('',#23147,#9355,#9356);
#7791=AXIS2_PLACEMENT_3D('',#23149,#9358,#9359);
#7792=AXIS2_PLACEMENT_3D('',#23150,#9360,#9361);
#7793=AXIS2_PLACEMENT_3D('',#23151,#9362,#9363);
#7794=AXIS2_PLACEMENT_3D('',#23153,#9364,#9365);
#7795=AXIS2_PLACEMENT_3D('',#23156,#9367,#9368);
#7796=AXIS2_PLACEMENT_3D('',#23157,#9369,#9370);
#7797=AXIS2_PLACEMENT_3D('',#23159,#9371,#9372);
#7798=AXIS2_PLACEMENT_3D('',#23162,#9374,#9375);
#7799=AXIS2_PLACEMENT_3D('',#23163,#9376,#9377);
#7800=AXIS2_PLACEMENT_3D('',#23168,#9379,#9380);
#7801=AXIS2_PLACEMENT_3D('',#23171,#9382,#9383);
#7802=AXIS2_PLACEMENT_3D('',#23172,#9384,#9385);
#7803=AXIS2_PLACEMENT_3D('',#23180,#9389,#9390);
#7804=AXIS2_PLACEMENT_3D('',#23186,#9394,#9395);
#7805=AXIS2_PLACEMENT_3D('',#23192,#9399,#9400);
#7806=AXIS2_PLACEMENT_3D('',#23196,#9403,#9404);
#7807=AXIS2_PLACEMENT_3D('',#23198,#9406,#9407);
#7808=AXIS2_PLACEMENT_3D('',#23202,#9410,#9411);
#7809=AXIS2_PLACEMENT_3D('',#23208,#9415,#9416);
#7810=AXIS2_PLACEMENT_3D('',#23210,#9418,#9419);
#7811=AXIS2_PLACEMENT_3D('',#23211,#9420,#9421);
#7812=AXIS2_PLACEMENT_3D('',#23212,#9422,#9423);
#7813=AXIS2_PLACEMENT_3D('',#23213,#9424,#9425);
#7814=AXIS2_PLACEMENT_3D('',#23214,#9426,#9427);
#7815=AXIS2_PLACEMENT_3D('',#23215,#9428,#9429);
#7816=AXIS2_PLACEMENT_3D('',#23216,#9430,#9431);
#7817=AXIS2_PLACEMENT_3D('',#23217,#9432,#9433);
#7818=AXIS2_PLACEMENT_3D('',#23218,#9434,#9435);
#7819=AXIS2_PLACEMENT_3D('',#23219,#9436,#9437);
#7820=AXIS2_PLACEMENT_3D('',#23220,#9438,#9439);
#7821=AXIS2_PLACEMENT_3D('',#23221,#9440,#9441);
#7822=AXIS2_PLACEMENT_3D('',#23222,#9442,#9443);
#7823=AXIS2_PLACEMENT_3D('',#23223,#9444,#9445);
#7824=AXIS2_PLACEMENT_3D('',#23224,#9446,#9447);
#7825=AXIS2_PLACEMENT_3D('',#23225,#9448,#9449);
#7826=AXIS2_PLACEMENT_3D('',#23226,#9450,#9451);
#7827=AXIS2_PLACEMENT_3D('',#23227,#9452,#9453);
#7828=AXIS2_PLACEMENT_3D('',#23228,#9454,#9455);
#7829=AXIS2_PLACEMENT_3D('',#23229,#9456,#9457);
#7830=AXIS2_PLACEMENT_3D('',#23230,#9458,#9459);
#7831=DIRECTION('axis',(0.,0.,1.));
#7832=DIRECTION('refdir',(1.,0.,0.));
#7833=DIRECTION('axis',(0.,0.,1.));
#7834=DIRECTION('refdir',(1.,0.,0.));
#7835=DIRECTION('center_axis',(0.,-1.,0.));
#7836=DIRECTION('ref_axis',(1.,0.,0.));
#7837=DIRECTION('center_axis',(0.,-1.,0.));
#7838=DIRECTION('ref_axis',(1.,0.,0.));
#7839=DIRECTION('',(0.,-1.,0.));
#7840=DIRECTION('center_axis',(0.,-1.,0.));
#7841=DIRECTION('ref_axis',(1.,0.,0.));
#7842=DIRECTION('center_axis',(0.,1.,0.));
#7843=DIRECTION('ref_axis',(0.,0.,1.));
#7844=DIRECTION('center_axis',(0.,-1.,0.));
#7845=DIRECTION('ref_axis',(1.,0.,0.));
#7846=DIRECTION('center_axis',(0.,-1.,0.));
#7847=DIRECTION('ref_axis',(1.,0.,0.));
#7848=DIRECTION('',(0.,-1.,0.));
#7849=DIRECTION('center_axis',(0.,-1.,0.));
#7850=DIRECTION('ref_axis',(1.,0.,0.));
#7851=DIRECTION('center_axis',(0.,-1.,0.));
#7852=DIRECTION('ref_axis',(0.,0.,-1.));
#7853=DIRECTION('center_axis',(0.,-1.,0.));
#7854=DIRECTION('ref_axis',(1.,0.,0.));
#7855=DIRECTION('center_axis',(0.,-1.,0.));
#7856=DIRECTION('ref_axis',(1.,0.,0.));
#7857=DIRECTION('',(0.,-1.,0.));
#7858=DIRECTION('center_axis',(0.,-1.,0.));
#7859=DIRECTION('ref_axis',(1.,0.,0.));
#7860=DIRECTION('center_axis',(0.,-1.,0.));
#7861=DIRECTION('ref_axis',(0.,0.,-1.));
#7862=DIRECTION('center_axis',(0.,-1.,0.));
#7863=DIRECTION('ref_axis',(1.,0.,0.));
#7864=DIRECTION('center_axis',(0.,-1.,0.));
#7865=DIRECTION('ref_axis',(1.,0.,0.));
#7866=DIRECTION('',(0.,-1.,0.));
#7867=DIRECTION('center_axis',(0.,-1.,0.));
#7868=DIRECTION('ref_axis',(1.,0.,0.));
#7869=DIRECTION('center_axis',(0.,1.,0.));
#7870=DIRECTION('ref_axis',(0.,0.,1.));
#7871=DIRECTION('center_axis',(0.,-1.,0.));
#7872=DIRECTION('ref_axis',(1.,0.,0.));
#7873=DIRECTION('center_axis',(0.,-1.,0.));
#7874=DIRECTION('ref_axis',(1.,0.,0.));
#7875=DIRECTION('',(0.,-1.,0.));
#7876=DIRECTION('center_axis',(0.,1.,0.));
#7877=DIRECTION('ref_axis',(1.,0.,0.));
#7878=DIRECTION('center_axis',(1.,0.,0.));
#7879=DIRECTION('ref_axis',(0.,1.,0.));
#7880=DIRECTION('center_axis',(1.,0.,0.));
#7881=DIRECTION('ref_axis',(0.,1.,0.));
#7882=DIRECTION('',(1.,0.,0.));
#7883=DIRECTION('center_axis',(1.,0.,0.));
#7884=DIRECTION('ref_axis',(0.,0.,-1.));
#7885=DIRECTION('center_axis',(-1.,0.,0.));
#7886=DIRECTION('ref_axis',(0.,0.,1.));
#7887=DIRECTION('center_axis',(1.,0.,0.));
#7888=DIRECTION('ref_axis',(0.,0.,-1.));
#7889=DIRECTION('center_axis',(1.,0.,0.));
#7890=DIRECTION('ref_axis',(0.,1.,0.));
#7891=DIRECTION('',(1.,0.,0.));
#7892=DIRECTION('center_axis',(1.,0.,0.));
#7893=DIRECTION('ref_axis',(0.,0.,-1.));
#7894=DIRECTION('center_axis',(1.,0.,0.));
#7895=DIRECTION('ref_axis',(0.,0.,-1.));
#7896=DIRECTION('center_axis',(1.,0.,0.));
#7897=DIRECTION('ref_axis',(0.,0.,-1.));
#7898=DIRECTION('center_axis',(1.,0.,0.));
#7899=DIRECTION('ref_axis',(0.,1.,0.));
#7900=DIRECTION('',(1.,0.,0.));
#7901=DIRECTION('center_axis',(1.,0.,0.));
#7902=DIRECTION('ref_axis',(0.,0.,-1.));
#7903=DIRECTION('center_axis',(1.,0.,0.));
#7904=DIRECTION('ref_axis',(0.,0.,-1.));
#7905=DIRECTION('center_axis',(1.,0.,0.));
#7906=DIRECTION('ref_axis',(0.,0.,-1.));
#7907=DIRECTION('center_axis',(1.,0.,0.));
#7908=DIRECTION('ref_axis',(0.,1.,0.));
#7909=DIRECTION('',(1.,0.,0.));
#7910=DIRECTION('center_axis',(-1.,0.,0.));
#7911=DIRECTION('ref_axis',(0.,1.,0.));
#7912=DIRECTION('center_axis',(1.,0.,0.));
#7913=DIRECTION('ref_axis',(0.,1.,0.));
#7914=DIRECTION('center_axis',(1.,0.,0.));
#7915=DIRECTION('ref_axis',(0.,1.,0.));
#7916=DIRECTION('',(1.,0.,0.));
#7917=DIRECTION('center_axis',(1.,0.,0.));
#7918=DIRECTION('ref_axis',(0.,0.,-1.));
#7919=DIRECTION('center_axis',(-1.,0.,0.));
#7920=DIRECTION('ref_axis',(0.,0.,1.));
#7921=DIRECTION('center_axis',(1.,0.,0.));
#7922=DIRECTION('ref_axis',(0.,0.,-1.));
#7923=DIRECTION('center_axis',(1.,0.,0.));
#7924=DIRECTION('ref_axis',(0.,1.,0.));
#7925=DIRECTION('',(1.,0.,0.));
#7926=DIRECTION('center_axis',(1.,0.,0.));
#7927=DIRECTION('ref_axis',(0.,0.,-1.));
#7928=DIRECTION('center_axis',(-1.,0.,0.));
#7929=DIRECTION('ref_axis',(0.,0.,1.));
#7930=DIRECTION('center_axis',(1.,0.,0.));
#7931=DIRECTION('ref_axis',(0.,0.,-1.));
#7932=DIRECTION('center_axis',(1.,0.,0.));
#7933=DIRECTION('ref_axis',(0.,1.,0.));
#7934=DIRECTION('',(1.,0.,0.));
#7935=DIRECTION('center_axis',(1.,0.,0.));
#7936=DIRECTION('ref_axis',(0.,0.,-1.));
#7937=DIRECTION('center_axis',(1.,0.,0.));
#7938=DIRECTION('ref_axis',(0.,0.,-1.));
#7939=DIRECTION('center_axis',(1.,0.,0.));
#7940=DIRECTION('ref_axis',(0.,0.,-1.));
#7941=DIRECTION('center_axis',(1.,0.,0.));
#7942=DIRECTION('ref_axis',(0.,1.,0.));
#7943=DIRECTION('',(1.,0.,0.));
#7944=DIRECTION('center_axis',(-1.,0.,0.));
#7945=DIRECTION('ref_axis',(0.,1.,0.));
#7946=DIRECTION('center_axis',(0.,-1.,0.));
#7947=DIRECTION('ref_axis',(0.,0.,-1.));
#7948=DIRECTION('center_axis',(0.,-1.,0.));
#7949=DIRECTION('ref_axis',(1.,0.,0.));
#7950=DIRECTION('center_axis',(-1.,0.,-1.22464679914735E-16));
#7951=DIRECTION('ref_axis',(-1.22464679914735E-16,0.,1.));
#7952=DIRECTION('center_axis',(0.,1.,0.));
#7953=DIRECTION('ref_axis',(1.,0.,0.));
#7954=DIRECTION('center_axis',(0.,-1.,0.));
#7955=DIRECTION('ref_axis',(1.,0.,0.));
#7956=DIRECTION('center_axis',(0.,-1.,0.));
#7957=DIRECTION('ref_axis',(1.,0.,0.));
#7958=DIRECTION('',(0.,1.,0.));
#7959=DIRECTION('center_axis',(0.,1.,0.));
#7960=DIRECTION('ref_axis',(-1.,0.,0.));
#7961=DIRECTION('center_axis',(0.,1.,0.));
#7962=DIRECTION('ref_axis',(-1.,0.,0.));
#7963=DIRECTION('center_axis',(0.,1.,0.));
#7964=DIRECTION('ref_axis',(-1.,0.,0.));
#7965=DIRECTION('',(1.,0.,0.));
#7966=DIRECTION('center_axis',(0.,-1.,0.));
#7967=DIRECTION('ref_axis',(-0.707106781186548,0.,-0.707106781186547));
#7968=DIRECTION('',(0.,0.,-1.));
#7969=DIRECTION('center_axis',(0.,-1.,0.));
#7970=DIRECTION('ref_axis',(-0.707106781186549,0.,0.707106781186546));
#7971=DIRECTION('',(-1.,0.,0.));
#7972=DIRECTION('center_axis',(0.,-1.,0.));
#7973=DIRECTION('ref_axis',(0.707106781186549,0.,0.707106781186546));
#7974=DIRECTION('',(0.,0.,1.));
#7975=DIRECTION('center_axis',(0.,-1.,0.));
#7976=DIRECTION('ref_axis',(0.707106781186548,0.,-0.707106781186547));
#7977=DIRECTION('center_axis',(0.,-1.,0.));
#7978=DIRECTION('ref_axis',(-1.,0.,0.));
#7979=DIRECTION('',(-0.707106781186549,0.707106781186546,-8.65956056235495E-17));
#7980=DIRECTION('center_axis',(0.,-1.,0.));
#7981=DIRECTION('ref_axis',(-1.,0.,0.));
#7982=DIRECTION('center_axis',(0.,1.,0.));
#7983=DIRECTION('ref_axis',(0.,0.,1.));
#7984=DIRECTION('center_axis',(0.,0.707106781186548,-0.707106781186548));
#7985=DIRECTION('ref_axis',(-1.,0.,0.));
#7986=DIRECTION('',(0.,0.707106781186548,0.707106781186548));
#7987=DIRECTION('',(0.,-0.707106781186548,-0.707106781186548));
#7988=DIRECTION('',(-1.,0.,0.));
#7989=DIRECTION('center_axis',(0.,-1.,0.));
#7990=DIRECTION('ref_axis',(-0.707106781186548,0.,-0.707106781186547));
#7991=DIRECTION('center_axis',(0.,1.,0.));
#7992=DIRECTION('ref_axis',(-0.707106781186548,0.,-0.707106781186547));
#7993=DIRECTION('',(0.707106781186545,0.70710678118655,0.));
#7994=DIRECTION('center_axis',(-0.707106781186548,0.707106781186548,0.));
#7995=DIRECTION('ref_axis',(0.,0.,1.));
#7996=DIRECTION('',(0.707106781186548,0.707106781186548,0.));
#7997=DIRECTION('',(0.,0.,1.));
#7998=DIRECTION('center_axis',(0.,-1.,0.));
#7999=DIRECTION('ref_axis',(-0.707106781186549,0.,0.707106781186546));
#8000=DIRECTION('center_axis',(0.,1.,0.));
#8001=DIRECTION('ref_axis',(-0.707106781186549,0.,0.707106781186546));
#8002=DIRECTION('',(0.,0.707106781186555,-0.70710678118654));
#8003=DIRECTION('center_axis',(0.,0.707106781186548,0.707106781186548));
#8004=DIRECTION('ref_axis',(1.,0.,0.));
#8005=DIRECTION('',(1.,0.,0.));
#8006=DIRECTION('',(0.,0.707106781186548,-0.707106781186548));
#8007=DIRECTION('center_axis',(0.,-1.,0.));
#8008=DIRECTION('ref_axis',(0.707106781186549,0.,0.707106781186546));
#8009=DIRECTION('center_axis',(0.,1.,0.));
#8010=DIRECTION('ref_axis',(0.707106781186549,0.,0.707106781186546));
#8011=DIRECTION('',(-0.707106781186549,0.707106781186546,0.));
#8012=DIRECTION('center_axis',(0.707106781186548,0.707106781186548,0.));
#8013=DIRECTION('ref_axis',(0.,0.,-1.));
#8014=DIRECTION('',(0.,0.,-1.));
#8015=DIRECTION('',(-0.707106781186548,0.707106781186548,0.));
#8016=DIRECTION('center_axis',(0.,-1.,0.));
#8017=DIRECTION('ref_axis',(0.707106781186548,0.,-0.707106781186547));
#8018=DIRECTION('center_axis',(0.,1.,0.));
#8019=DIRECTION('ref_axis',(0.707106781186548,0.,-0.707106781186547));
#8020=DIRECTION('center_axis',(0.,-1.,0.));
#8021=DIRECTION('ref_axis',(-0.707106781186549,0.,0.707106781186546));
#8022=DIRECTION('',(0.,-1.,0.));
#8023=DIRECTION('center_axis',(0.,-1.,0.));
#8024=DIRECTION('ref_axis',(-0.707106781186549,0.,0.707106781186546));
#8025=DIRECTION('',(0.,1.,0.));
#8026=DIRECTION('center_axis',(-1.,0.,0.));
#8027=DIRECTION('ref_axis',(0.,-1.,0.));
#8028=DIRECTION('',(0.,1.,0.));
#8029=DIRECTION('',(0.,0.,-1.));
#8030=DIRECTION('center_axis',(0.,-1.,0.));
#8031=DIRECTION('ref_axis',(-0.707106781186548,0.,-0.707106781186547));
#8032=DIRECTION('',(0.,-1.,0.));
#8033=DIRECTION('center_axis',(0.,-1.,0.));
#8034=DIRECTION('ref_axis',(-0.707106781186548,0.,-0.707106781186547));
#8035=DIRECTION('center_axis',(0.,0.,1.));
#8036=DIRECTION('ref_axis',(1.,0.,0.));
#8037=DIRECTION('',(0.,1.,0.));
#8038=DIRECTION('',(1.,0.,0.));
#8039=DIRECTION('center_axis',(0.,1.,0.));
#8040=DIRECTION('ref_axis',(-0.707106781186549,0.,0.707106781186546));
#8041=DIRECTION('',(0.,0.707106781186554,0.707106781186541));
#8042=DIRECTION('',(0.707106781186549,-0.707106781186546,0.));
#8043=DIRECTION('center_axis',(0.,1.,0.));
#8044=DIRECTION('ref_axis',(-0.707106781186549,0.,0.707106781186546));
#8045=DIRECTION('center_axis',(0.,-0.707106781186546,0.707106781186549));
#8046=DIRECTION('ref_axis',(1.,0.,0.));
#8047=DIRECTION('',(0.,0.707106781186549,0.707106781186546));
#8048=DIRECTION('',(-1.,0.,0.));
#8049=DIRECTION('',(1.,0.,0.));
#8050=DIRECTION('center_axis',(0.,1.,0.));
#8051=DIRECTION('ref_axis',(0.707106781186549,0.,0.707106781186546));
#8052=DIRECTION('',(0.707106781186547,0.707106781186547,0.));
#8053=DIRECTION('center_axis',(0.,-1.,0.));
#8054=DIRECTION('ref_axis',(0.707106781186549,0.,0.707106781186546));
#8055=DIRECTION('center_axis',(0.,1.,0.));
#8056=DIRECTION('ref_axis',(0.707106781186549,0.,0.707106781186546));
#8057=DIRECTION('center_axis',(0.707106781186549,-0.707106781186546,0.));
#8058=DIRECTION('ref_axis',(0.,0.,-1.));
#8059=DIRECTION('',(0.,0.,-1.));
#8060=DIRECTION('',(0.707106781186546,0.707106781186549,0.));
#8061=DIRECTION('',(0.,0.,1.));
#8062=DIRECTION('center_axis',(0.,1.,0.));
#8063=DIRECTION('ref_axis',(0.707106781186548,0.,-0.707106781186547));
#8064=DIRECTION('',(0.,0.707106781186549,-0.707106781186546));
#8065=DIRECTION('center_axis',(0.,-1.,0.));
#8066=DIRECTION('ref_axis',(0.707106781186548,0.,-0.707106781186547));
#8067=DIRECTION('center_axis',(0.,1.,0.));
#8068=DIRECTION('ref_axis',(0.707106781186548,0.,-0.707106781186547));
#8069=DIRECTION('center_axis',(0.,-0.707106781186548,-0.707106781186548));
#8070=DIRECTION('ref_axis',(-1.,0.,0.));
#8071=DIRECTION('',(-1.,0.,0.));
#8072=DIRECTION('',(0.,0.707106781186546,-0.707106781186549));
#8073=DIRECTION('center_axis',(0.,1.,0.));
#8074=DIRECTION('ref_axis',(-0.707106781186548,0.,-0.707106781186547));
#8075=DIRECTION('',(-0.707106781186549,0.707106781186546,0.));
#8076=DIRECTION('center_axis',(0.,1.,0.));
#8077=DIRECTION('ref_axis',(-0.707106781186548,0.,-0.707106781186547));
#8078=DIRECTION('center_axis',(-0.707106781186548,-0.707106781186547,0.));
#8079=DIRECTION('ref_axis',(0.,0.,1.));
#8080=DIRECTION('',(0.,0.,1.));
#8081=DIRECTION('center_axis',(0.,-1.,0.));
#8082=DIRECTION('ref_axis',(1.,0.,0.));
#8083=DIRECTION('center_axis',(0.,-1.,0.));
#8084=DIRECTION('ref_axis',(-0.707106781186546,0.,0.707106781186549));
#8085=DIRECTION('',(-1.,0.,0.));
#8086=DIRECTION('center_axis',(0.,-1.,0.));
#8087=DIRECTION('ref_axis',(0.707106781186546,0.,0.707106781186549));
#8088=DIRECTION('',(0.,0.,1.));
#8089=DIRECTION('center_axis',(0.,-1.,0.));
#8090=DIRECTION('ref_axis',(0.707106781186548,0.,-0.707106781186548));
#8091=DIRECTION('',(1.,0.,0.));
#8092=DIRECTION('center_axis',(0.,-1.,0.));
#8093=DIRECTION('ref_axis',(-0.707106781186548,0.,-0.707106781186548));
#8094=DIRECTION('',(0.,0.,-1.));
#8095=DIRECTION('center_axis',(0.,-1.,0.));
#8096=DIRECTION('ref_axis',(-0.707106781186546,0.,0.707106781186549));
#8097=DIRECTION('',(0.707106781186547,0.707106781186547,6.28036983473509E-15));
#8098=DIRECTION('center_axis',(0.,1.,0.));
#8099=DIRECTION('ref_axis',(-0.707106781186546,0.,0.707106781186549));
#8100=DIRECTION('',(0.,-0.707106781186549,0.707106781186546));
#8101=DIRECTION('center_axis',(0.707106781186548,-0.707106781186547,0.));
#8102=DIRECTION('ref_axis',(0.,0.,-1.));
#8103=DIRECTION('',(0.707106781186547,0.707106781186547,0.));
#8104=DIRECTION('',(0.,0.,1.));
#8105=DIRECTION('center_axis',(0.,-1.,0.));
#8106=DIRECTION('ref_axis',(-0.707106781186548,0.,-0.707106781186548));
#8107=DIRECTION('',(0.,0.707106781186549,0.707106781186546));
#8108=DIRECTION('center_axis',(0.,1.,0.));
#8109=DIRECTION('ref_axis',(-0.707106781186547,0.,-0.707106781186547));
#8110=DIRECTION('center_axis',(0.,-0.707106781186548,0.707106781186548));
#8111=DIRECTION('ref_axis',(1.,0.,0.));
#8112=DIRECTION('',(0.,0.707106781186547,0.707106781186547));
#8113=DIRECTION('',(-1.,0.,0.));
#8114=DIRECTION('center_axis',(0.,-1.,0.));
#8115=DIRECTION('ref_axis',(0.707106781186548,0.,-0.707106781186548));
#8116=DIRECTION('',(-0.707106781186546,0.707106781186549,0.));
#8117=DIRECTION('center_axis',(0.,1.,0.));
#8118=DIRECTION('ref_axis',(0.707106781186547,0.,-0.707106781186547));
#8119=DIRECTION('center_axis',(-0.707106781186546,-0.707106781186549,0.));
#8120=DIRECTION('ref_axis',(0.,0.,1.));
#8121=DIRECTION('',(-0.707106781186549,0.707106781186546,0.));
#8122=DIRECTION('',(0.,0.,-1.));
#8123=DIRECTION('center_axis',(0.,-1.,0.));
#8124=DIRECTION('ref_axis',(0.707106781186546,0.,0.707106781186549));
#8125=DIRECTION('',(0.,0.707106781186549,-0.707106781186546));
#8126=DIRECTION('center_axis',(0.,1.,0.));
#8127=DIRECTION('ref_axis',(0.707106781186546,0.,0.707106781186549));
#8128=DIRECTION('center_axis',(0.,-0.707106781186546,-0.707106781186549));
#8129=DIRECTION('ref_axis',(-1.,0.,0.));
#8130=DIRECTION('',(1.,0.,0.));
#8131=DIRECTION('center_axis',(1.,0.,0.));
#8132=DIRECTION('ref_axis',(0.,1.,0.));
#8133=DIRECTION('',(0.,-1.,0.));
#8134=DIRECTION('',(0.,0.,1.));
#8135=DIRECTION('',(0.,1.,0.));
#8136=DIRECTION('center_axis',(0.,1.,0.));
#8137=DIRECTION('ref_axis',(0.707106781186546,0.,0.707106781186549));
#8138=DIRECTION('',(0.,1.,0.));
#8139=DIRECTION('center_axis',(0.,-1.,0.));
#8140=DIRECTION('ref_axis',(0.707106781186546,0.,0.707106781186549));
#8141=DIRECTION('center_axis',(0.,0.,1.));
#8142=DIRECTION('ref_axis',(1.,0.,0.));
#8143=DIRECTION('',(0.,-1.,0.));
#8144=DIRECTION('',(-1.,0.,0.));
#8145=DIRECTION('center_axis',(0.,-1.,0.));
#8146=DIRECTION('ref_axis',(-0.707106781186546,0.,0.707106781186549));
#8147=DIRECTION('',(0.,1.,0.));
#8148=DIRECTION('center_axis',(0.,-1.,0.));
#8149=DIRECTION('ref_axis',(-0.707106781186546,0.,0.707106781186549));
#8150=DIRECTION('center_axis',(0.,1.,0.));
#8151=DIRECTION('ref_axis',(-1.,0.,0.));
#8152=DIRECTION('',(0.,0.,1.));
#8153=DIRECTION('center_axis',(0.,-1.,0.));
#8154=DIRECTION('ref_axis',(-0.707106781186547,0.,-0.707106781186547));
#8155=DIRECTION('',(-1.,0.,0.));
#8156=DIRECTION('center_axis',(0.,-1.,0.));
#8157=DIRECTION('ref_axis',(0.707106781186547,0.,-0.707106781186547));
#8158=DIRECTION('center_axis',(-1.,0.,0.));
#8159=DIRECTION('ref_axis',(0.,-1.,0.));
#8160=DIRECTION('',(0.,-1.,0.));
#8161=DIRECTION('center_axis',(0.,-1.,0.));
#8162=DIRECTION('ref_axis',(-0.707106781186547,0.,-0.707106781186547));
#8163=DIRECTION('',(0.,1.,0.));
#8164=DIRECTION('center_axis',(0.,1.,0.));
#8165=DIRECTION('ref_axis',(0.707106781186547,0.,-0.707106781186547));
#8166=DIRECTION('',(0.,-1.,0.));
#8167=DIRECTION('center_axis',(0.,0.,1.));
#8168=DIRECTION('ref_axis',(1.,0.,0.));
#8169=DIRECTION('center_axis',(0.,1.,0.));
#8170=DIRECTION('ref_axis',(0.707106781186549,0.,0.707106781186546));
#8171=DIRECTION('',(0.,-1.,0.));
#8172=DIRECTION('',(0.,1.,0.));
#8173=DIRECTION('center_axis',(1.,0.,0.));
#8174=DIRECTION('ref_axis',(0.,1.,0.));
#8175=DIRECTION('',(0.,-1.,0.));
#8176=DIRECTION('center_axis',(0.,1.,0.));
#8177=DIRECTION('ref_axis',(0.707106781186548,0.,-0.707106781186547));
#8178=DIRECTION('center_axis',(0.,0.,1.));
#8179=DIRECTION('ref_axis',(1.,0.,0.));
#8180=DIRECTION('axis',(0.,0.,1.));
#8181=DIRECTION('refdir',(1.,0.,0.));
#8182=DIRECTION('center_axis',(1.,0.,0.));
#8183=DIRECTION('ref_axis',(0.,1.,0.));
#8184=DIRECTION('',(-0.739012155113086,0.673692091830617,8.2503486387125E-17));
#8185=DIRECTION('center_axis',(1.,0.,0.));
#8186=DIRECTION('ref_axis',(0.,0.,-1.));
#8187=DIRECTION('center_axis',(0.,-1.,0.));
#8188=DIRECTION('ref_axis',(0.,0.,-1.));
#8189=DIRECTION('',(-8.65956056235493E-17,0.707106781186548,-0.707106781186547));
#8190=DIRECTION('center_axis',(0.,1.,0.));
#8191=DIRECTION('ref_axis',(0.,0.,-1.));
#8192=DIRECTION('center_axis',(0.,1.,0.));
#8193=DIRECTION('ref_axis',(0.,0.,-1.));
#8194=DIRECTION('',(0.,1.,0.));
#8195=DIRECTION('center_axis',(0.,0.,1.));
#8196=DIRECTION('ref_axis',(1.,0.,0.));
#8197=DIRECTION('',(0.707106781186547,-8.65956056235493E-17,-0.707106781186548));
#8198=DIRECTION('center_axis',(0.,0.,-1.));
#8199=DIRECTION('ref_axis',(1.,0.,0.));
#8200=DIRECTION('center_axis',(0.,0.,-1.));
#8201=DIRECTION('ref_axis',(1.,0.,0.));
#8202=DIRECTION('',(0.,0.,-1.));
#8203=DIRECTION('center_axis',(-1.,0.,0.));
#8204=DIRECTION('ref_axis',(0.,-1.,0.));
#8205=DIRECTION('center_axis',(-1.,0.,0.));
#8206=DIRECTION('ref_axis',(0.,-1.,0.));
#8207=DIRECTION('',(0.707106781186547,-0.707106781186547,8.65956056235493E-17));
#8208=DIRECTION('center_axis',(1.,0.,0.));
#8209=DIRECTION('ref_axis',(0.,-1.,0.));
#8210=DIRECTION('center_axis',(1.,0.,0.));
#8211=DIRECTION('ref_axis',(0.,-1.,0.));
#8212=DIRECTION('center_axis',(1.,0.,0.));
#8213=DIRECTION('ref_axis',(0.,1.,0.));
#8214=DIRECTION('center_axis',(-1.,0.,0.));
#8215=DIRECTION('ref_axis',(0.,-1.,0.));
#8216=DIRECTION('center_axis',(-1.,0.,0.));
#8217=DIRECTION('ref_axis',(0.,-1.,0.));
#8218=DIRECTION('',(-1.,0.,0.));
#8219=DIRECTION('',(-1.,0.,0.));
#8220=DIRECTION('center_axis',(-1.,0.,0.));
#8221=DIRECTION('ref_axis',(0.,0.,1.));
#8222=DIRECTION('center_axis',(1.,0.,0.));
#8223=DIRECTION('ref_axis',(0.,0.,-1.));
#8224=DIRECTION('center_axis',(1.,0.,0.));
#8225=DIRECTION('ref_axis',(0.,0.,-1.));
#8226=DIRECTION('center_axis',(1.,0.,0.));
#8227=DIRECTION('ref_axis',(0.,0.,-1.));
#8228=DIRECTION('center_axis',(1.,0.,0.));
#8229=DIRECTION('ref_axis',(0.,0.,-1.));
#8230=DIRECTION('center_axis',(1.,0.,0.));
#8231=DIRECTION('ref_axis',(0.,0.,-1.));
#8232=DIRECTION('center_axis',(1.,0.,0.));
#8233=DIRECTION('ref_axis',(0.,0.,-1.));
#8234=DIRECTION('center_axis',(1.,0.,0.));
#8235=DIRECTION('ref_axis',(0.,0.,-1.));
#8236=DIRECTION('center_axis',(1.,0.,0.));
#8237=DIRECTION('ref_axis',(0.,0.,-1.));
#8238=DIRECTION('center_axis',(1.,0.,0.));
#8239=DIRECTION('ref_axis',(0.,0.,-1.));
#8240=DIRECTION('center_axis',(1.,0.,0.));
#8241=DIRECTION('ref_axis',(0.,0.,-1.));
#8242=DIRECTION('center_axis',(1.,0.,0.));
#8243=DIRECTION('ref_axis',(0.,0.,-1.));
#8244=DIRECTION('center_axis',(1.,0.,0.));
#8245=DIRECTION('ref_axis',(0.,0.,-1.));
#8246=DIRECTION('center_axis',(1.,0.,0.));
#8247=DIRECTION('ref_axis',(0.,0.,-1.));
#8248=DIRECTION('center_axis',(1.,0.,0.));
#8249=DIRECTION('ref_axis',(0.,0.,-1.));
#8250=DIRECTION('center_axis',(1.,0.,0.));
#8251=DIRECTION('ref_axis',(0.,0.,-1.));
#8252=DIRECTION('center_axis',(1.,0.,0.));
#8253=DIRECTION('ref_axis',(0.,0.,-1.));
#8254=DIRECTION('center_axis',(1.,0.,0.));
#8255=DIRECTION('ref_axis',(0.,0.,-1.));
#8256=DIRECTION('center_axis',(1.,0.,0.));
#8257=DIRECTION('ref_axis',(0.,0.,-1.));
#8258=DIRECTION('center_axis',(1.,0.,0.));
#8259=DIRECTION('ref_axis',(0.,0.,-1.));
#8260=DIRECTION('center_axis',(1.,0.,0.));
#8261=DIRECTION('ref_axis',(0.,-1.,0.));
#8262=DIRECTION('',(0.707106781186546,0.707106781186549,-8.65956056235495E-17));
#8263=DIRECTION('center_axis',(1.,0.,0.));
#8264=DIRECTION('ref_axis',(0.,-1.,0.));
#8265=DIRECTION('center_axis',(1.,0.,0.));
#8266=DIRECTION('ref_axis',(0.,0.,-1.));
#8267=DIRECTION('center_axis',(-1.,0.,0.));
#8268=DIRECTION('ref_axis',(0.,-1.,0.));
#8269=DIRECTION('center_axis',(-1.,0.,0.));
#8270=DIRECTION('ref_axis',(0.,-1.,0.));
#8271=DIRECTION('',(-0.707106781186546,0.707106781186549,8.65956056235495E-17));
#8272=DIRECTION('center_axis',(1.,0.,0.));
#8273=DIRECTION('ref_axis',(0.,-1.,0.));
#8274=DIRECTION('center_axis',(1.,0.,0.));
#8275=DIRECTION('ref_axis',(0.,-1.,0.));
#8276=DIRECTION('center_axis',(1.,0.,0.));
#8277=DIRECTION('ref_axis',(0.,1.,0.));
#8278=DIRECTION('',(-1.,0.,0.));
#8279=DIRECTION('',(-1.,0.,0.));
#8280=DIRECTION('center_axis',(1.,0.,0.));
#8281=DIRECTION('ref_axis',(0.,0.,-1.));
#8282=DIRECTION('center_axis',(-1.,0.,0.));
#8283=DIRECTION('ref_axis',(0.,1.,0.));
#8284=DIRECTION('center_axis',(1.,-9.71851396181453E-17,-2.16484527094502E-17));
#8285=DIRECTION('ref_axis',(0.,1.,0.));
#8286=DIRECTION('center_axis',(-1.,0.,0.));
#8287=DIRECTION('ref_axis',(0.,1.,0.));
#8288=DIRECTION('center_axis',(1.,-8.57388205317489E-17,-5.0620761759739E-17));
#8289=DIRECTION('ref_axis',(0.,1.,0.));
#8290=DIRECTION('center_axis',(-1.,0.,0.));
#8291=DIRECTION('ref_axis',(0.,1.,0.));
#8292=DIRECTION('center_axis',(1.,-6.58997883142157E-17,-7.46379579533984E-17));
#8293=DIRECTION('ref_axis',(0.,1.,0.));
#8294=DIRECTION('center_axis',(-1.,0.,0.));
#8295=DIRECTION('ref_axis',(0.,1.,0.));
#8296=DIRECTION('center_axis',(1.,-3.96100256656632E-17,-9.13490707893474E-17));
#8297=DIRECTION('ref_axis',(0.,1.,0.));
#8298=DIRECTION('center_axis',(-1.,0.,0.));
#8299=DIRECTION('ref_axis',(0.,1.,0.));
#8300=DIRECTION('center_axis',(1.,-9.44295772567882E-18,-9.91183001100339E-17));
#8301=DIRECTION('ref_axis',(0.,1.,0.));
#8302=DIRECTION('center_axis',(-1.,0.,0.));
#8303=DIRECTION('ref_axis',(0.,1.,0.));
#8304=DIRECTION('center_axis',(1.,2.16484527094502E-17,-9.71851396181453E-17));
#8305=DIRECTION('ref_axis',(0.,1.,0.));
#8306=DIRECTION('center_axis',(-1.,0.,0.));
#8307=DIRECTION('ref_axis',(0.,1.,0.));
#8308=DIRECTION('center_axis',(1.,5.0620761759739E-17,-8.57388205317489E-17));
#8309=DIRECTION('ref_axis',(0.,1.,0.));
#8310=DIRECTION('center_axis',(-1.,0.,0.));
#8311=DIRECTION('ref_axis',(0.,1.,0.));
#8312=DIRECTION('center_axis',(1.,7.46379579533984E-17,-6.58997883142157E-17));
#8313=DIRECTION('ref_axis',(0.,1.,0.));
#8314=DIRECTION('center_axis',(-1.,0.,0.));
#8315=DIRECTION('ref_axis',(0.,1.,0.));
#8316=DIRECTION('center_axis',(1.,9.13490707893474E-17,-3.96100256656632E-17));
#8317=DIRECTION('ref_axis',(0.,1.,0.));
#8318=DIRECTION('center_axis',(-1.,0.,0.));
#8319=DIRECTION('ref_axis',(0.,-0.997421223023649,0.0717697977007645));
#8320=DIRECTION('center_axis',(1.,9.91183001100339E-17,-9.44295772567882E-18));
#8321=DIRECTION('ref_axis',(0.,1.,0.));
#8322=DIRECTION('center_axis',(-1.,0.,0.));
#8323=DIRECTION('ref_axis',(0.,1.,0.));
#8324=DIRECTION('center_axis',(1.,9.71851396181453E-17,2.16484527094502E-17));
#8325=DIRECTION('ref_axis',(0.,1.,0.));
#8326=DIRECTION('center_axis',(-1.,0.,0.));
#8327=DIRECTION('ref_axis',(0.,1.,0.));
#8328=DIRECTION('center_axis',(1.,8.57388205317489E-17,5.0620761759739E-17));
#8329=DIRECTION('ref_axis',(0.,1.,0.));
#8330=DIRECTION('center_axis',(-1.,0.,0.));
#8331=DIRECTION('ref_axis',(0.,1.,0.));
#8332=DIRECTION('center_axis',(1.,6.58997883142157E-17,7.46379579533984E-17));
#8333=DIRECTION('ref_axis',(0.,1.,0.));
#8334=DIRECTION('center_axis',(-1.,0.,0.));
#8335=DIRECTION('ref_axis',(0.,1.,0.));
#8336=DIRECTION('center_axis',(1.,3.96100256656632E-17,9.13490707893474E-17));
#8337=DIRECTION('ref_axis',(0.,1.,0.));
#8338=DIRECTION('center_axis',(-1.,0.,0.));
#8339=DIRECTION('ref_axis',(0.,1.,0.));
#8340=DIRECTION('center_axis',(1.,9.44295772567883E-18,9.91183001100339E-17));
#8341=DIRECTION('ref_axis',(0.,1.,0.));
#8342=DIRECTION('center_axis',(-1.,0.,0.));
#8343=DIRECTION('ref_axis',(0.,1.,0.));
#8344=DIRECTION('center_axis',(1.,-2.16484527094502E-17,9.71851396181453E-17));
#8345=DIRECTION('ref_axis',(0.,1.,0.));
#8346=DIRECTION('center_axis',(-1.,0.,0.));
#8347=DIRECTION('ref_axis',(0.,1.,0.));
#8348=DIRECTION('center_axis',(1.,-5.0620761759739E-17,8.57388205317489E-17));
#8349=DIRECTION('ref_axis',(0.,1.,0.));
#8350=DIRECTION('center_axis',(-1.,0.,0.));
#8351=DIRECTION('ref_axis',(0.,1.,0.));
#8352=DIRECTION('center_axis',(1.,-7.46379579533983E-17,6.58997883142157E-17));
#8353=DIRECTION('ref_axis',(0.,1.,0.));
#8354=DIRECTION('center_axis',(-1.,0.,0.));
#8355=DIRECTION('ref_axis',(0.,1.,0.));
#8356=DIRECTION('center_axis',(1.,-9.13490707893474E-17,3.96100256656632E-17));
#8357=DIRECTION('ref_axis',(0.,1.,0.));
#8358=DIRECTION('center_axis',(-1.,0.,0.));
#8359=DIRECTION('ref_axis',(0.,1.,0.));
#8360=DIRECTION('center_axis',(-1.,0.,0.));
#8361=DIRECTION('ref_axis',(0.,1.,0.));
#8362=DIRECTION('',(0.68394112888133,0.729537204140085,8.93425401909064E-17));
#8363=DIRECTION('center_axis',(1.,0.,0.));
#8364=DIRECTION('ref_axis',(0.,0.,-1.));
#8365=DIRECTION('center_axis',(1.,0.,0.));
#8366=DIRECTION('ref_axis',(0.,1.,0.));
#8367=DIRECTION('',(1.,0.,0.));
#8368=DIRECTION('center_axis',(1.,0.,0.));
#8369=DIRECTION('ref_axis',(0.,1.,0.));
#8370=DIRECTION('center_axis',(-1.,0.,0.));
#8371=DIRECTION('ref_axis',(0.,1.,0.));
#8372=DIRECTION('center_axis',(1.,-9.91183001100339E-17,9.44295772567884E-18));
#8373=DIRECTION('ref_axis',(0.,1.,0.));
#8374=DIRECTION('',(0.657420344909251,0.731109352828835,0.182421501763368));
#8375=DIRECTION('',(0.657420344909251,0.751697658316477,-0.0524320568061806));
#8376=DIRECTION('',(0.657420344909251,0.698704559622551,-0.28215320033992));
#8377=DIRECTION('',(0.657420344909251,0.577317390471848,-0.484255222747444));
#8378=DIRECTION('',(0.657420344909251,0.399418372734979,-0.638954969947916));
#8379=DIRECTION('',(0.657420344909251,0.182421501763368,-0.731109352828835));
#8380=DIRECTION('',(0.657420344909251,-0.0524320568061806,-0.751697658316477));
#8381=DIRECTION('',(0.657420344909251,-0.282153200339919,-0.698704559622551));
#8382=DIRECTION('',(0.657420344909251,-0.484255222747444,-0.577317390471848));
#8383=DIRECTION('',(0.657420344909251,-0.638954969947916,-0.399418372734979));
#8384=DIRECTION('',(0.657420344909251,-0.731109352828835,-0.182421501763368));
#8385=DIRECTION('',(0.657420344909251,-0.751697658316477,0.0524320568061806));
#8386=DIRECTION('',(0.657420344909251,-0.698704559622551,0.282153200339919));
#8387=DIRECTION('',(0.657420344909251,-0.577317390471848,0.484255222747444));
#8388=DIRECTION('',(0.657420344909251,-0.399418372734979,0.638954969947916));
#8389=DIRECTION('',(0.657420344909251,-0.182421501763368,0.731109352828835));
#8390=DIRECTION('',(0.657420344909251,0.0524320568061804,0.751697658316477));
#8391=DIRECTION('',(0.657420344909251,0.282153200339919,0.698704559622551));
#8392=DIRECTION('',(0.657420344909251,0.484255222747444,0.577317390471848));
#8393=DIRECTION('',(0.657420344909251,0.638954969947916,0.399418372734979));
#8394=DIRECTION('center_axis',(1.,-9.91183001100339E-17,9.44295772567884E-18));
#8395=DIRECTION('ref_axis',(-2.16484527094502E-17,-0.309016994374948,-0.951056516295153));
#8396=DIRECTION('center_axis',(1.,-9.91183001100339E-17,9.44295772567884E-18));
#8397=DIRECTION('ref_axis',(0.,1.,0.));
#8398=DIRECTION('center_axis',(1.,0.,0.));
#8399=DIRECTION('ref_axis',(0.,1.,0.));
#8400=DIRECTION('',(-0.739012155113086,0.673692091830617,8.2503486387125E-17));
#8401=DIRECTION('center_axis',(1.,9.91183001100339E-17,-9.44295772567882E-18));
#8402=DIRECTION('ref_axis',(0.,1.,0.));
#8403=DIRECTION('center_axis',(1.,9.71851396181453E-17,2.16484527094502E-17));
#8404=DIRECTION('ref_axis',(0.,1.,0.));
#8405=DIRECTION('center_axis',(1.,8.57388205317489E-17,5.0620761759739E-17));
#8406=DIRECTION('ref_axis',(0.,1.,0.));
#8407=DIRECTION('center_axis',(1.,6.58997883142157E-17,7.46379579533984E-17));
#8408=DIRECTION('ref_axis',(0.,1.,0.));
#8409=DIRECTION('center_axis',(1.,3.96100256656632E-17,9.13490707893474E-17));
#8410=DIRECTION('ref_axis',(0.,1.,0.));
#8411=DIRECTION('center_axis',(1.,9.44295772567883E-18,9.91183001100339E-17));
#8412=DIRECTION('ref_axis',(0.,1.,0.));
#8413=DIRECTION('center_axis',(1.,-2.16484527094502E-17,9.71851396181453E-17));
#8414=DIRECTION('ref_axis',(0.,1.,0.));
#8415=DIRECTION('center_axis',(1.,-5.0620761759739E-17,8.57388205317489E-17));
#8416=DIRECTION('ref_axis',(0.,1.,0.));
#8417=DIRECTION('center_axis',(1.,-7.46379579533983E-17,6.58997883142157E-17));
#8418=DIRECTION('ref_axis',(0.,1.,0.));
#8419=DIRECTION('center_axis',(1.,-9.13490707893474E-17,3.96100256656632E-17));
#8420=DIRECTION('ref_axis',(0.,1.,0.));
#8421=DIRECTION('center_axis',(1.,-9.71851396181453E-17,-2.16484527094502E-17));
#8422=DIRECTION('ref_axis',(0.,1.,0.));
#8423=DIRECTION('center_axis',(1.,-8.57388205317489E-17,-5.0620761759739E-17));
#8424=DIRECTION('ref_axis',(0.,1.,0.));
#8425=DIRECTION('center_axis',(1.,-6.58997883142157E-17,-7.46379579533984E-17));
#8426=DIRECTION('ref_axis',(0.,1.,0.));
#8427=DIRECTION('center_axis',(1.,-3.96100256656632E-17,-9.13490707893474E-17));
#8428=DIRECTION('ref_axis',(0.,1.,0.));
#8429=DIRECTION('center_axis',(1.,-9.44295772567882E-18,-9.91183001100339E-17));
#8430=DIRECTION('ref_axis',(0.,1.,0.));
#8431=DIRECTION('center_axis',(1.,2.16484527094502E-17,-9.71851396181453E-17));
#8432=DIRECTION('ref_axis',(0.,1.,0.));
#8433=DIRECTION('center_axis',(1.,5.0620761759739E-17,-8.57388205317489E-17));
#8434=DIRECTION('ref_axis',(0.,1.,0.));
#8435=DIRECTION('center_axis',(1.,7.46379579533984E-17,-6.58997883142157E-17));
#8436=DIRECTION('ref_axis',(0.,1.,0.));
#8437=DIRECTION('center_axis',(1.,9.13490707893474E-17,-3.96100256656632E-17));
#8438=DIRECTION('ref_axis',(0.,1.,0.));
#8439=DIRECTION('center_axis',(1.,9.91183001100339E-17,-9.44295772567882E-18));
#8440=DIRECTION('ref_axis',(0.,1.,0.));
#8441=DIRECTION('center_axis',(1.,-9.13490707893474E-17,3.96100256656632E-17));
#8442=DIRECTION('ref_axis',(-2.16484527094502E-17,-0.587785252292473,-0.809016994374947));
#8443=DIRECTION('center_axis',(1.,-7.46379579533983E-17,6.58997883142157E-17));
#8444=DIRECTION('ref_axis',(-2.16484527094502E-17,-0.809016994374948,-0.587785252292473));
#8445=DIRECTION('center_axis',(1.,-5.0620761759739E-17,8.57388205317489E-17));
#8446=DIRECTION('ref_axis',(-2.16484527094502E-17,-0.951056516295154,-0.309016994374947));
#8447=DIRECTION('center_axis',(1.,-2.16484527094502E-17,9.71851396181453E-17));
#8448=DIRECTION('ref_axis',(-2.16484527094502E-17,-1.,1.83697019872103E-16));
#8449=DIRECTION('center_axis',(1.,9.44295772567883E-18,9.91183001100339E-17));
#8450=DIRECTION('ref_axis',(-2.16484527094502E-17,-0.951056516295153,0.309016994374948));
#8451=DIRECTION('center_axis',(1.,3.96100256656632E-17,9.13490707893474E-17));
#8452=DIRECTION('ref_axis',(-2.16484527094502E-17,-0.809016994374947,0.587785252292473));
#8453=DIRECTION('center_axis',(1.,6.58997883142157E-17,7.46379579533984E-17));
#8454=DIRECTION('ref_axis',(-2.16484527094502E-17,-0.587785252292473,0.809016994374947));
#8455=DIRECTION('center_axis',(1.,8.57388205317489E-17,5.0620761759739E-17));
#8456=DIRECTION('ref_axis',(-2.16484527094502E-17,-0.309016994374947,0.951056516295154));
#8457=DIRECTION('center_axis',(1.,9.71851396181453E-17,2.16484527094502E-17));
#8458=DIRECTION('ref_axis',(-2.16484527094502E-17,1.22464679914735E-16,
1.));
#8459=DIRECTION('center_axis',(1.,9.91183001100339E-17,-9.44295772567882E-18));
#8460=DIRECTION('ref_axis',(-2.16484527094502E-17,0.309016994374948,0.951056516295153));
#8461=DIRECTION('center_axis',(1.,9.13490707893474E-17,-3.96100256656632E-17));
#8462=DIRECTION('ref_axis',(-2.16484527094502E-17,0.587785252292473,0.809016994374947));
#8463=DIRECTION('center_axis',(1.,7.46379579533984E-17,-6.58997883142157E-17));
#8464=DIRECTION('ref_axis',(-2.16484527094502E-17,0.809016994374947,0.587785252292473));
#8465=DIRECTION('center_axis',(1.,5.0620761759739E-17,-8.57388205317489E-17));
#8466=DIRECTION('ref_axis',(-2.16484527094502E-17,0.951056516295154,0.309016994374947));
#8467=DIRECTION('center_axis',(1.,2.16484527094502E-17,-9.71851396181453E-17));
#8468=DIRECTION('ref_axis',(-2.16484527094502E-17,1.,-6.12323399573677E-17));
#8469=DIRECTION('center_axis',(1.,-9.44295772567882E-18,-9.91183001100339E-17));
#8470=DIRECTION('ref_axis',(-2.16484527094502E-17,0.951056516295154,-0.309016994374948));
#8471=DIRECTION('center_axis',(1.,-3.96100256656632E-17,-9.13490707893474E-17));
#8472=DIRECTION('ref_axis',(-2.16484527094502E-17,0.809016994374947,-0.587785252292473));
#8473=DIRECTION('center_axis',(1.,-6.58997883142157E-17,-7.46379579533984E-17));
#8474=DIRECTION('ref_axis',(-2.16484527094502E-17,0.587785252292473,-0.809016994374947));
#8475=DIRECTION('center_axis',(1.,-8.57388205317489E-17,-5.0620761759739E-17));
#8476=DIRECTION('ref_axis',(-2.16484527094502E-17,0.309016994374947,-0.951056516295154));
#8477=DIRECTION('center_axis',(1.,-9.71851396181453E-17,-2.16484527094502E-17));
#8478=DIRECTION('ref_axis',(-2.16484527094502E-17,0.,-1.));
#8479=DIRECTION('center_axis',(1.,0.,0.));
#8480=DIRECTION('ref_axis',(0.,0.,-1.));
#8481=DIRECTION('axis',(0.,0.,1.));
#8482=DIRECTION('refdir',(1.,0.,0.));
#8483=DIRECTION('center_axis',(0.,-1.,0.));
#8484=DIRECTION('ref_axis',(0.,0.,-1.));
#8485=DIRECTION('',(-8.65956056235493E-17,0.707106781186548,-0.707106781186547));
#8486=DIRECTION('center_axis',(0.,1.,0.));
#8487=DIRECTION('ref_axis',(0.,0.,-1.));
#8488=DIRECTION('center_axis',(0.,1.,0.));
#8489=DIRECTION('ref_axis',(0.,0.,-1.));
#8490=DIRECTION('',(0.,1.,0.));
#8491=DIRECTION('center_axis',(0.,0.,1.));
#8492=DIRECTION('ref_axis',(1.,0.,0.));
#8493=DIRECTION('',(0.707106781186547,-8.65956056235493E-17,-0.707106781186548));
#8494=DIRECTION('center_axis',(0.,0.,-1.));
#8495=DIRECTION('ref_axis',(1.,0.,0.));
#8496=DIRECTION('center_axis',(0.,0.,-1.));
#8497=DIRECTION('ref_axis',(1.,0.,0.));
#8498=DIRECTION('',(0.,0.,-1.));
#8499=DIRECTION('center_axis',(-1.,0.,0.));
#8500=DIRECTION('ref_axis',(0.,-1.,0.));
#8501=DIRECTION('center_axis',(-1.,0.,0.));
#8502=DIRECTION('ref_axis',(0.,-1.,0.));
#8503=DIRECTION('',(0.707106781186547,-0.707106781186547,8.65956056235493E-17));
#8504=DIRECTION('center_axis',(1.,0.,0.));
#8505=DIRECTION('ref_axis',(0.,-1.,0.));
#8506=DIRECTION('center_axis',(1.,0.,0.));
#8507=DIRECTION('ref_axis',(0.,-1.,0.));
#8508=DIRECTION('center_axis',(1.,0.,0.));
#8509=DIRECTION('ref_axis',(0.,1.,0.));
#8510=DIRECTION('center_axis',(-1.,0.,0.));
#8511=DIRECTION('ref_axis',(0.,-1.,0.));
#8512=DIRECTION('center_axis',(-1.,0.,0.));
#8513=DIRECTION('ref_axis',(0.,-1.,0.));
#8514=DIRECTION('',(-1.,0.,0.));
#8515=DIRECTION('',(-1.,0.,0.));
#8516=DIRECTION('center_axis',(-1.,0.,0.));
#8517=DIRECTION('ref_axis',(0.,0.,1.));
#8518=DIRECTION('center_axis',(1.,0.,0.));
#8519=DIRECTION('ref_axis',(0.,0.,-1.));
#8520=DIRECTION('center_axis',(1.,0.,0.));
#8521=DIRECTION('ref_axis',(0.,0.,-1.));
#8522=DIRECTION('center_axis',(1.,0.,0.));
#8523=DIRECTION('ref_axis',(0.,0.,-1.));
#8524=DIRECTION('center_axis',(1.,0.,0.));
#8525=DIRECTION('ref_axis',(0.,0.,-1.));
#8526=DIRECTION('center_axis',(1.,0.,0.));
#8527=DIRECTION('ref_axis',(0.,0.,-1.));
#8528=DIRECTION('center_axis',(1.,0.,0.));
#8529=DIRECTION('ref_axis',(0.,0.,-1.));
#8530=DIRECTION('center_axis',(1.,0.,0.));
#8531=DIRECTION('ref_axis',(0.,0.,-1.));
#8532=DIRECTION('center_axis',(1.,0.,0.));
#8533=DIRECTION('ref_axis',(0.,0.,-1.));
#8534=DIRECTION('center_axis',(1.,0.,0.));
#8535=DIRECTION('ref_axis',(0.,0.,-1.));
#8536=DIRECTION('center_axis',(1.,0.,0.));
#8537=DIRECTION('ref_axis',(0.,0.,-1.));
#8538=DIRECTION('center_axis',(1.,0.,0.));
#8539=DIRECTION('ref_axis',(0.,0.,-1.));
#8540=DIRECTION('center_axis',(1.,0.,0.));
#8541=DIRECTION('ref_axis',(0.,0.,-1.));
#8542=DIRECTION('center_axis',(1.,0.,0.));
#8543=DIRECTION('ref_axis',(0.,0.,-1.));
#8544=DIRECTION('center_axis',(1.,0.,0.));
#8545=DIRECTION('ref_axis',(0.,0.,-1.));
#8546=DIRECTION('center_axis',(1.,0.,0.));
#8547=DIRECTION('ref_axis',(0.,0.,-1.));
#8548=DIRECTION('center_axis',(1.,0.,0.));
#8549=DIRECTION('ref_axis',(0.,0.,-1.));
#8550=DIRECTION('center_axis',(1.,0.,0.));
#8551=DIRECTION('ref_axis',(0.,0.,-1.));
#8552=DIRECTION('center_axis',(1.,0.,0.));
#8553=DIRECTION('ref_axis',(0.,0.,-1.));
#8554=DIRECTION('center_axis',(1.,0.,0.));
#8555=DIRECTION('ref_axis',(0.,0.,-1.));
#8556=DIRECTION('center_axis',(1.,0.,0.));
#8557=DIRECTION('ref_axis',(0.,0.,-1.));
#8558=DIRECTION('center_axis',(1.,0.,0.));
#8559=DIRECTION('ref_axis',(0.,-1.,0.));
#8560=DIRECTION('',(0.707106781186546,0.707106781186549,-8.65956056235495E-17));
#8561=DIRECTION('center_axis',(1.,0.,0.));
#8562=DIRECTION('ref_axis',(0.,-1.,0.));
#8563=DIRECTION('center_axis',(1.,0.,0.));
#8564=DIRECTION('ref_axis',(0.,0.,-1.));
#8565=DIRECTION('center_axis',(-1.,0.,0.));
#8566=DIRECTION('ref_axis',(0.,-1.,0.));
#8567=DIRECTION('center_axis',(-1.,0.,0.));
#8568=DIRECTION('ref_axis',(0.,-1.,0.));
#8569=DIRECTION('',(-0.707106781186546,0.707106781186549,8.65956056235495E-17));
#8570=DIRECTION('center_axis',(1.,0.,0.));
#8571=DIRECTION('ref_axis',(0.,-1.,0.));
#8572=DIRECTION('center_axis',(1.,0.,0.));
#8573=DIRECTION('ref_axis',(0.,-1.,0.));
#8574=DIRECTION('center_axis',(1.,0.,0.));
#8575=DIRECTION('ref_axis',(0.,1.,0.));
#8576=DIRECTION('',(-1.,0.,0.));
#8577=DIRECTION('',(-1.,0.,0.));
#8578=DIRECTION('center_axis',(1.,0.,0.));
#8579=DIRECTION('ref_axis',(0.,0.,-1.));
#8580=DIRECTION('center_axis',(-1.,0.,0.));
#8581=DIRECTION('ref_axis',(0.,1.,0.));
#8582=DIRECTION('center_axis',(1.,-9.89384015765324E-17,1.11713723763385E-17));
#8583=DIRECTION('ref_axis',(0.,1.,0.));
#8584=DIRECTION('center_axis',(-1.,0.,0.));
#8585=DIRECTION('ref_axis',(0.,1.,0.));
#8586=DIRECTION('center_axis',(1.,-9.75481554459673E-17,-1.99490409889652E-17));
#8587=DIRECTION('ref_axis',(0.,1.,0.));
#8588=DIRECTION('center_axis',(-1.,0.,0.));
#8589=DIRECTION('ref_axis',(0.,1.,0.));
#8590=DIRECTION('center_axis',(1.,-8.66092162023871E-17,-4.91167032291274E-17));
#8591=DIRECTION('ref_axis',(0.,1.,0.));
#8592=DIRECTION('center_axis',(-1.,0.,0.));
#8593=DIRECTION('ref_axis',(0.,1.,0.));
#8594=DIRECTION('center_axis',(1.,-6.71923634350248E-17,-7.34764803410285E-17));
#8595=DIRECTION('ref_axis',(0.,1.,0.));
#8596=DIRECTION('center_axis',(-1.,0.,0.));
#8597=DIRECTION('ref_axis',(0.,1.,0.));
#8598=DIRECTION('center_axis',(1.,-4.1198253977918E-17,-9.06438676164084E-17));
#8599=DIRECTION('ref_axis',(0.,1.,0.));
#8600=DIRECTION('center_axis',(-1.,0.,0.));
#8601=DIRECTION('ref_axis',(0.,1.,0.));
#8602=DIRECTION('center_axis',(1.,-1.11713723763385E-17,-9.89384015765324E-17));
#8603=DIRECTION('ref_axis',(0.,1.,0.));
#8604=DIRECTION('center_axis',(-1.,0.,0.));
#8605=DIRECTION('ref_axis',(0.,1.,0.));
#8606=DIRECTION('center_axis',(1.,1.99490409889652E-17,-9.75481554459673E-17));
#8607=DIRECTION('ref_axis',(0.,1.,0.));
#8608=DIRECTION('center_axis',(-1.,0.,0.));
#8609=DIRECTION('ref_axis',(0.,1.,0.));
#8610=DIRECTION('center_axis',(1.,4.91167032291274E-17,-8.66092162023871E-17));
#8611=DIRECTION('ref_axis',(0.,1.,0.));
#8612=DIRECTION('center_axis',(-1.,0.,0.));
#8613=DIRECTION('ref_axis',(0.,1.,0.));
#8614=DIRECTION('center_axis',(1.,7.34764803410285E-17,-6.71923634350248E-17));
#8615=DIRECTION('ref_axis',(0.,1.,0.));
#8616=DIRECTION('center_axis',(-1.,0.,0.));
#8617=DIRECTION('ref_axis',(0.,1.,0.));
#8618=DIRECTION('center_axis',(1.,9.06438676164084E-17,-4.1198253977918E-17));
#8619=DIRECTION('ref_axis',(0.,1.,0.));
#8620=DIRECTION('center_axis',(-1.,0.,0.));
#8621=DIRECTION('ref_axis',(0.,-0.996349796141496,0.0853644172287271));
#8622=DIRECTION('center_axis',(1.,9.89384015765324E-17,-1.11713723763385E-17));
#8623=DIRECTION('ref_axis',(0.,1.,0.));
#8624=DIRECTION('center_axis',(-1.,0.,0.));
#8625=DIRECTION('ref_axis',(0.,1.,0.));
#8626=DIRECTION('center_axis',(1.,9.75481554459673E-17,1.99490409889651E-17));
#8627=DIRECTION('ref_axis',(0.,1.,0.));
#8628=DIRECTION('center_axis',(-1.,0.,0.));
#8629=DIRECTION('ref_axis',(0.,1.,0.));
#8630=DIRECTION('center_axis',(1.,8.66092162023871E-17,4.91167032291274E-17));
#8631=DIRECTION('ref_axis',(0.,1.,0.));
#8632=DIRECTION('center_axis',(-1.,0.,0.));
#8633=DIRECTION('ref_axis',(0.,1.,0.));
#8634=DIRECTION('center_axis',(1.,6.71923634350248E-17,7.34764803410285E-17));
#8635=DIRECTION('ref_axis',(0.,1.,0.));
#8636=DIRECTION('center_axis',(-1.,0.,0.));
#8637=DIRECTION('ref_axis',(0.,1.,0.));
#8638=DIRECTION('center_axis',(1.,4.1198253977918E-17,9.06438676164084E-17));
#8639=DIRECTION('ref_axis',(0.,1.,0.));
#8640=DIRECTION('center_axis',(-1.,0.,0.));
#8641=DIRECTION('ref_axis',(0.,1.,0.));
#8642=DIRECTION('center_axis',(1.,1.11713723763385E-17,9.89384015765324E-17));
#8643=DIRECTION('ref_axis',(0.,1.,0.));
#8644=DIRECTION('center_axis',(-1.,0.,0.));
#8645=DIRECTION('ref_axis',(0.,1.,0.));
#8646=DIRECTION('center_axis',(1.,-1.99490409889651E-17,9.75481554459673E-17));
#8647=DIRECTION('ref_axis',(0.,1.,0.));
#8648=DIRECTION('center_axis',(-1.,0.,0.));
#8649=DIRECTION('ref_axis',(0.,1.,0.));
#8650=DIRECTION('center_axis',(1.,-4.91167032291274E-17,8.66092162023871E-17));
#8651=DIRECTION('ref_axis',(0.,1.,0.));
#8652=DIRECTION('center_axis',(-1.,0.,0.));
#8653=DIRECTION('ref_axis',(0.,1.,0.));
#8654=DIRECTION('center_axis',(1.,-7.34764803410285E-17,6.71923634350248E-17));
#8655=DIRECTION('ref_axis',(0.,1.,0.));
#8656=DIRECTION('center_axis',(-1.,0.,0.));
#8657=DIRECTION('ref_axis',(0.,1.,0.));
#8658=DIRECTION('center_axis',(-1.,0.,0.));
#8659=DIRECTION('ref_axis',(0.,1.,0.));
#8660=DIRECTION('',(0.68394112888133,0.729537204140085,8.93425401909064E-17));
#8661=DIRECTION('center_axis',(1.,0.,0.));
#8662=DIRECTION('ref_axis',(0.,0.,-1.));
#8663=DIRECTION('center_axis',(1.,0.,0.));
#8664=DIRECTION('ref_axis',(0.,1.,0.));
#8665=DIRECTION('',(1.,0.,0.));
#8666=DIRECTION('center_axis',(1.,0.,0.));
#8667=DIRECTION('ref_axis',(0.,1.,0.));
#8668=DIRECTION('center_axis',(-1.,0.,0.));
#8669=DIRECTION('ref_axis',(0.,1.,0.));
#8670=DIRECTION('center_axis',(1.,-9.06438676164084E-17,4.11982539779181E-17));
#8671=DIRECTION('ref_axis',(0.,1.,0.));
#8672=DIRECTION('',(0.657420344909251,0.594324098593915,-0.46322495175663));
#8673=DIRECTION('',(0.657420344909251,0.422091424447672,-0.624209355510742));
#8674=DIRECTION('',(0.657420344909251,0.20854150079261,-0.724091798425149));
#8675=DIRECTION('',(0.657420344909251,-0.0254219179541074,-0.753095091065488));
#8676=DIRECTION('',(0.657420344909251,-0.256896862246559,-0.7083801890703));
#8677=DIRECTION('',(0.657420344909251,-0.463224951756629,-0.594324098593915));
#8678=DIRECTION('',(0.657420344909251,-0.624209355510742,-0.422091424447672));
#8679=DIRECTION('',(0.657420344909251,-0.724091798425149,-0.20854150079261));
#8680=DIRECTION('',(0.657420344909251,-0.753095091065488,0.0254219179541074));
#8681=DIRECTION('',(0.657420344909251,-0.7083801890703,0.256896862246559));
#8682=DIRECTION('',(0.657420344909251,-0.594324098593915,0.463224951756629));
#8683=DIRECTION('',(0.657420344909251,-0.422091424447672,0.624209355510742));
#8684=DIRECTION('',(0.657420344909251,-0.20854150079261,0.724091798425149));
#8685=DIRECTION('',(0.657420344909251,0.0254219179541074,0.753095091065488));
#8686=DIRECTION('',(0.657420344909251,0.256896862246559,0.7083801890703));
#8687=DIRECTION('',(0.657420344909251,0.463224951756629,0.594324098593915));
#8688=DIRECTION('',(0.657420344909251,0.624209355510742,0.422091424447673));
#8689=DIRECTION('',(0.657420344909251,0.724091798425149,0.20854150079261));
#8690=DIRECTION('',(0.657420344909251,0.753095091065488,-0.0254219179541073));
#8691=DIRECTION('',(0.657420344909251,0.7083801890703,-0.256896862246559));
#8692=DIRECTION('center_axis',(1.,-9.06438676164084E-17,4.11982539779181E-17));
#8693=DIRECTION('ref_axis',(1.11713723763385E-17,-0.309016994374948,-0.951056516295153));
#8694=DIRECTION('center_axis',(1.,-9.06438676164084E-17,4.11982539779181E-17));
#8695=DIRECTION('ref_axis',(0.,1.,0.));
#8696=DIRECTION('center_axis',(1.,0.,0.));
#8697=DIRECTION('ref_axis',(0.,1.,0.));
#8698=DIRECTION('',(-0.739012155113086,0.673692091830617,8.2503486387125E-17));
#8699=DIRECTION('center_axis',(1.,9.89384015765324E-17,-1.11713723763385E-17));
#8700=DIRECTION('ref_axis',(0.,1.,0.));
#8701=DIRECTION('center_axis',(1.,9.75481554459673E-17,1.99490409889651E-17));
#8702=DIRECTION('ref_axis',(0.,1.,0.));
#8703=DIRECTION('center_axis',(1.,8.66092162023871E-17,4.91167032291274E-17));
#8704=DIRECTION('ref_axis',(0.,1.,0.));
#8705=DIRECTION('center_axis',(1.,6.71923634350248E-17,7.34764803410285E-17));
#8706=DIRECTION('ref_axis',(0.,1.,0.));
#8707=DIRECTION('center_axis',(1.,4.1198253977918E-17,9.06438676164084E-17));
#8708=DIRECTION('ref_axis',(0.,1.,0.));
#8709=DIRECTION('center_axis',(1.,1.11713723763385E-17,9.89384015765324E-17));
#8710=DIRECTION('ref_axis',(0.,1.,0.));
#8711=DIRECTION('center_axis',(1.,-1.99490409889651E-17,9.75481554459673E-17));
#8712=DIRECTION('ref_axis',(0.,1.,0.));
#8713=DIRECTION('center_axis',(1.,-4.91167032291274E-17,8.66092162023871E-17));
#8714=DIRECTION('ref_axis',(0.,1.,0.));
#8715=DIRECTION('center_axis',(1.,-7.34764803410285E-17,6.71923634350248E-17));
#8716=DIRECTION('ref_axis',(0.,1.,0.));
#8717=DIRECTION('center_axis',(1.,-9.89384015765324E-17,1.11713723763385E-17));
#8718=DIRECTION('ref_axis',(0.,1.,0.));
#8719=DIRECTION('center_axis',(1.,-9.75481554459673E-17,-1.99490409889652E-17));
#8720=DIRECTION('ref_axis',(0.,1.,0.));
#8721=DIRECTION('center_axis',(1.,-8.66092162023871E-17,-4.91167032291274E-17));
#8722=DIRECTION('ref_axis',(0.,1.,0.));
#8723=DIRECTION('center_axis',(1.,-6.71923634350248E-17,-7.34764803410285E-17));
#8724=DIRECTION('ref_axis',(0.,1.,0.));
#8725=DIRECTION('center_axis',(1.,-4.1198253977918E-17,-9.06438676164084E-17));
#8726=DIRECTION('ref_axis',(0.,1.,0.));
#8727=DIRECTION('center_axis',(1.,-1.11713723763385E-17,-9.89384015765324E-17));
#8728=DIRECTION('ref_axis',(0.,1.,0.));
#8729=DIRECTION('center_axis',(1.,1.99490409889652E-17,-9.75481554459673E-17));
#8730=DIRECTION('ref_axis',(0.,1.,0.));
#8731=DIRECTION('center_axis',(1.,4.91167032291274E-17,-8.66092162023871E-17));
#8732=DIRECTION('ref_axis',(0.,1.,0.));
#8733=DIRECTION('center_axis',(1.,7.34764803410285E-17,-6.71923634350248E-17));
#8734=DIRECTION('ref_axis',(0.,1.,0.));
#8735=DIRECTION('center_axis',(1.,9.06438676164084E-17,-4.1198253977918E-17));
#8736=DIRECTION('ref_axis',(0.,1.,0.));
#8737=DIRECTION('center_axis',(1.,9.89384015765324E-17,-1.11713723763385E-17));
#8738=DIRECTION('ref_axis',(0.,1.,0.));
#8739=DIRECTION('center_axis',(1.,-7.34764803410285E-17,6.71923634350248E-17));
#8740=DIRECTION('ref_axis',(1.11713723763385E-17,-0.587785252292473,-0.809016994374947));
#8741=DIRECTION('center_axis',(1.,-4.91167032291274E-17,8.66092162023871E-17));
#8742=DIRECTION('ref_axis',(1.11713723763385E-17,-0.809016994374948,-0.587785252292473));
#8743=DIRECTION('center_axis',(1.,-1.99490409889651E-17,9.75481554459673E-17));
#8744=DIRECTION('ref_axis',(1.11713723763385E-17,-0.951056516295154,-0.309016994374947));
#8745=DIRECTION('center_axis',(1.,1.11713723763385E-17,9.89384015765324E-17));
#8746=DIRECTION('ref_axis',(1.11713723763385E-17,-1.,1.83697019872103E-16));
#8747=DIRECTION('center_axis',(1.,4.1198253977918E-17,9.06438676164084E-17));
#8748=DIRECTION('ref_axis',(1.11713723763385E-17,-0.951056516295153,0.309016994374948));
#8749=DIRECTION('center_axis',(1.,6.71923634350248E-17,7.34764803410285E-17));
#8750=DIRECTION('ref_axis',(1.11713723763385E-17,-0.809016994374947,0.587785252292473));
#8751=DIRECTION('center_axis',(1.,8.66092162023871E-17,4.91167032291274E-17));
#8752=DIRECTION('ref_axis',(1.11713723763385E-17,-0.587785252292473,0.809016994374947));
#8753=DIRECTION('center_axis',(1.,9.75481554459673E-17,1.99490409889651E-17));
#8754=DIRECTION('ref_axis',(1.11713723763385E-17,-0.309016994374947,0.951056516295154));
#8755=DIRECTION('center_axis',(1.,9.89384015765324E-17,-1.11713723763385E-17));
#8756=DIRECTION('ref_axis',(1.11713723763385E-17,1.22464679914735E-16,1.));
#8757=DIRECTION('center_axis',(1.,9.06438676164084E-17,-4.1198253977918E-17));
#8758=DIRECTION('ref_axis',(1.11713723763385E-17,0.309016994374948,0.951056516295153));
#8759=DIRECTION('center_axis',(1.,7.34764803410285E-17,-6.71923634350248E-17));
#8760=DIRECTION('ref_axis',(1.11713723763385E-17,0.587785252292473,0.809016994374947));
#8761=DIRECTION('center_axis',(1.,4.91167032291274E-17,-8.66092162023871E-17));
#8762=DIRECTION('ref_axis',(1.11713723763385E-17,0.809016994374947,0.587785252292473));
#8763=DIRECTION('center_axis',(1.,1.99490409889652E-17,-9.75481554459673E-17));
#8764=DIRECTION('ref_axis',(1.11713723763385E-17,0.951056516295154,0.309016994374947));
#8765=DIRECTION('center_axis',(1.,-1.11713723763385E-17,-9.89384015765324E-17));
#8766=DIRECTION('ref_axis',(1.11713723763385E-17,1.,-6.12323399573677E-17));
#8767=DIRECTION('center_axis',(1.,-4.1198253977918E-17,-9.06438676164084E-17));
#8768=DIRECTION('ref_axis',(1.11713723763385E-17,0.951056516295154,-0.309016994374948));
#8769=DIRECTION('center_axis',(1.,-6.71923634350248E-17,-7.34764803410285E-17));
#8770=DIRECTION('ref_axis',(1.11713723763385E-17,0.809016994374947,-0.587785252292473));
#8771=DIRECTION('center_axis',(1.,-8.66092162023871E-17,-4.91167032291274E-17));
#8772=DIRECTION('ref_axis',(1.11713723763385E-17,0.587785252292473,-0.809016994374947));
#8773=DIRECTION('center_axis',(1.,-9.75481554459673E-17,-1.99490409889652E-17));
#8774=DIRECTION('ref_axis',(1.11713723763385E-17,0.309016994374947,-0.951056516295154));
#8775=DIRECTION('center_axis',(1.,-9.89384015765324E-17,1.11713723763385E-17));
#8776=DIRECTION('ref_axis',(1.11713723763385E-17,0.,-1.));
#8777=DIRECTION('center_axis',(1.,0.,0.));
#8778=DIRECTION('ref_axis',(0.,0.,-1.));
#8779=DIRECTION('axis',(0.,0.,1.));
#8780=DIRECTION('refdir',(1.,0.,0.));
#8781=DIRECTION('center_axis',(-1.,0.,0.));
#8782=DIRECTION('ref_axis',(0.,0.,1.));
#8783=DIRECTION('center_axis',(-1.,0.,0.));
#8784=DIRECTION('ref_axis',(0.,1.,0.));
#8785=DIRECTION('',(0.,0.,1.));
#8786=DIRECTION('center_axis',(-1.,0.,0.));
#8787=DIRECTION('ref_axis',(0.,1.,0.));
#8788=DIRECTION('center_axis',(1.,0.,0.));
#8789=DIRECTION('ref_axis',(0.,0.,-1.));
#8790=DIRECTION('center_axis',(1.,0.,0.));
#8791=DIRECTION('ref_axis',(0.,1.,0.));
#8792=DIRECTION('',(0.,0.,-1.));
#8793=DIRECTION('center_axis',(1.,0.,0.));
#8794=DIRECTION('ref_axis',(0.,1.,0.));
#8795=DIRECTION('center_axis',(0.,1.,0.));
#8796=DIRECTION('ref_axis',(0.,0.,1.));
#8797=DIRECTION('',(-1.,0.,0.));
#8798=DIRECTION('',(1.,0.,0.));
#8799=DIRECTION('center_axis',(-1.,0.,0.));
#8800=DIRECTION('ref_axis',(0.,-1.,0.));
#8801=DIRECTION('center_axis',(-1.,0.,0.));
#8802=DIRECTION('ref_axis',(0.,1.,0.));
#8803=DIRECTION('',(0.,1.,0.));
#8804=DIRECTION('center_axis',(0.,0.,-1.));
#8805=DIRECTION('ref_axis',(-1.,0.,0.));
#8806=DIRECTION('',(-1.,0.,0.));
#8807=DIRECTION('',(0.,-1.,0.));
#8808=DIRECTION('',(1.,0.,0.));
#8809=DIRECTION('center_axis',(1.,0.,0.));
#8810=DIRECTION('ref_axis',(0.,1.,0.));
#8811=DIRECTION('center_axis',(1.,0.,0.));
#8812=DIRECTION('ref_axis',(0.,1.,0.));
#8813=DIRECTION('center_axis',(1.,0.,0.));
#8814=DIRECTION('ref_axis',(0.,1.,0.));
#8815=DIRECTION('',(0.499772441725887,-0.866156744758906,-1.06073608502889E-16));
#8816=DIRECTION('center_axis',(1.,0.,0.));
#8817=DIRECTION('ref_axis',(0.,0.,-1.));
#8818=DIRECTION('center_axis',(1.,0.,0.));
#8819=DIRECTION('ref_axis',(0.,1.,0.));
#8820=DIRECTION('',(1.,0.,0.));
#8821=DIRECTION('center_axis',(-1.,0.,0.));
#8822=DIRECTION('ref_axis',(0.,1.,0.));
#8823=DIRECTION('center_axis',(1.,0.,0.));
#8824=DIRECTION('ref_axis',(0.,1.,0.));
#8825=DIRECTION('center_axis',(1.,0.,0.));
#8826=DIRECTION('ref_axis',(0.,1.,0.));
#8827=DIRECTION('',(1.,0.,0.));
#8828=DIRECTION('center_axis',(1.,0.,0.));
#8829=DIRECTION('ref_axis',(0.,0.,-1.));
#8830=DIRECTION('center_axis',(-1.,0.,0.));
#8831=DIRECTION('ref_axis',(0.,1.,0.));
#8832=DIRECTION('',(0.499772441725888,0.866156744758905,1.06073608502888E-16));
#8833=DIRECTION('center_axis',(-1.,0.,0.));
#8834=DIRECTION('ref_axis',(0.,0.,1.));
#8835=DIRECTION('center_axis',(1.,0.,0.));
#8836=DIRECTION('ref_axis',(0.,0.,-1.));
#8837=DIRECTION('center_axis',(1.,0.,0.));
#8838=DIRECTION('ref_axis',(0.,1.,0.));
#8839=DIRECTION('center_axis',(1.,0.,0.));
#8840=DIRECTION('ref_axis',(0.,0.,-1.));
#8841=DIRECTION('',(-0.707106781186548,0.707106781186547,8.65956056235493E-17));
#8842=DIRECTION('center_axis',(1.,0.,0.));
#8843=DIRECTION('ref_axis',(0.,1.,0.));
#8844=DIRECTION('center_axis',(1.,0.,0.));
#8845=DIRECTION('ref_axis',(0.,0.,-1.));
#8846=DIRECTION('',(-1.,0.,0.));
#8847=DIRECTION('',(-1.,0.,0.));
#8848=DIRECTION('center_axis',(-1.,0.,0.));
#8849=DIRECTION('ref_axis',(0.,1.,0.));
#8850=DIRECTION('center_axis',(1.,0.,0.));
#8851=DIRECTION('ref_axis',(0.,0.,-1.));
#8852=DIRECTION('',(-0.707106781186548,-0.707106781186547,-8.65956056235493E-17));
#8853=DIRECTION('center_axis',(1.,0.,0.));
#8854=DIRECTION('ref_axis',(0.,0.,-1.));
#8855=DIRECTION('axis',(0.,0.,1.));
#8856=DIRECTION('refdir',(1.,0.,0.));
#8857=DIRECTION('center_axis',(-1.,0.,0.));
#8858=DIRECTION('ref_axis',(0.,0.,1.));
#8859=DIRECTION('center_axis',(-1.,0.,0.));
#8860=DIRECTION('ref_axis',(0.,1.,0.));
#8861=DIRECTION('',(0.,0.,1.));
#8862=DIRECTION('center_axis',(-1.,0.,0.));
#8863=DIRECTION('ref_axis',(0.,1.,0.));
#8864=DIRECTION('center_axis',(1.,0.,0.));
#8865=DIRECTION('ref_axis',(0.,0.,-1.));
#8866=DIRECTION('center_axis',(1.,0.,0.));
#8867=DIRECTION('ref_axis',(0.,1.,0.));
#8868=DIRECTION('',(0.,0.,-1.));
#8869=DIRECTION('center_axis',(1.,0.,0.));
#8870=DIRECTION('ref_axis',(0.,1.,0.));
#8871=DIRECTION('center_axis',(0.,1.,0.));
#8872=DIRECTION('ref_axis',(0.,0.,1.));
#8873=DIRECTION('',(-1.,0.,0.));
#8874=DIRECTION('',(1.,0.,0.));
#8875=DIRECTION('center_axis',(-1.,0.,0.));
#8876=DIRECTION('ref_axis',(0.,-1.,0.));
#8877=DIRECTION('center_axis',(-1.,0.,0.));
#8878=DIRECTION('ref_axis',(0.,1.,0.));
#8879=DIRECTION('',(0.,1.,0.));
#8880=DIRECTION('center_axis',(0.,0.,-1.));
#8881=DIRECTION('ref_axis',(-1.,0.,0.));
#8882=DIRECTION('',(-1.,0.,0.));
#8883=DIRECTION('',(0.,-1.,0.));
#8884=DIRECTION('',(1.,0.,0.));
#8885=DIRECTION('center_axis',(1.,0.,0.));
#8886=DIRECTION('ref_axis',(0.,1.,0.));
#8887=DIRECTION('center_axis',(1.,0.,0.));
#8888=DIRECTION('ref_axis',(0.,1.,0.));
#8889=DIRECTION('center_axis',(1.,0.,0.));
#8890=DIRECTION('ref_axis',(0.,1.,0.));
#8891=DIRECTION('',(0.499772441725887,-0.866156744758906,-1.06073608502889E-16));
#8892=DIRECTION('center_axis',(1.,0.,0.));
#8893=DIRECTION('ref_axis',(0.,0.,-1.));
#8894=DIRECTION('center_axis',(1.,0.,0.));
#8895=DIRECTION('ref_axis',(0.,1.,0.));
#8896=DIRECTION('',(1.,0.,0.));
#8897=DIRECTION('center_axis',(-1.,0.,0.));
#8898=DIRECTION('ref_axis',(0.,1.,0.));
#8899=DIRECTION('center_axis',(1.,0.,0.));
#8900=DIRECTION('ref_axis',(0.,1.,0.));
#8901=DIRECTION('center_axis',(1.,0.,0.));
#8902=DIRECTION('ref_axis',(0.,1.,0.));
#8903=DIRECTION('',(1.,0.,0.));
#8904=DIRECTION('center_axis',(1.,0.,0.));
#8905=DIRECTION('ref_axis',(0.,0.,-1.));
#8906=DIRECTION('center_axis',(-1.,0.,0.));
#8907=DIRECTION('ref_axis',(0.,1.,0.));
#8908=DIRECTION('',(0.499772441725887,0.866156744758906,1.06073608502889E-16));
#8909=DIRECTION('center_axis',(-1.,0.,0.));
#8910=DIRECTION('ref_axis',(0.,0.,1.));
#8911=DIRECTION('center_axis',(1.,0.,0.));
#8912=DIRECTION('ref_axis',(0.,0.,-1.));
#8913=DIRECTION('center_axis',(1.,0.,0.));
#8914=DIRECTION('ref_axis',(0.,1.,0.));
#8915=DIRECTION('center_axis',(1.,0.,0.));
#8916=DIRECTION('ref_axis',(0.,0.,-1.));
#8917=DIRECTION('',(-0.707106781186548,0.707106781186547,8.65956056235493E-17));
#8918=DIRECTION('center_axis',(1.,0.,0.));
#8919=DIRECTION('ref_axis',(0.,1.,0.));
#8920=DIRECTION('center_axis',(1.,0.,0.));
#8921=DIRECTION('ref_axis',(0.,0.,-1.));
#8922=DIRECTION('',(-1.,0.,0.));
#8923=DIRECTION('',(-1.,0.,0.));
#8924=DIRECTION('center_axis',(-1.,0.,0.));
#8925=DIRECTION('ref_axis',(0.,1.,0.));
#8926=DIRECTION('center_axis',(1.,0.,0.));
#8927=DIRECTION('ref_axis',(0.,0.,-1.));
#8928=DIRECTION('',(-0.707106781186548,-0.707106781186547,-8.65956056235493E-17));
#8929=DIRECTION('center_axis',(1.,0.,0.));
#8930=DIRECTION('ref_axis',(0.,0.,-1.));
#8931=DIRECTION('axis',(0.,0.,1.));
#8932=DIRECTION('refdir',(1.,0.,0.));
#8933=DIRECTION('center_axis',(0.,0.587785252292474,0.809016994374947));
#8934=DIRECTION('ref_axis',(1.,0.,0.));
#8935=DIRECTION('center_axis',(0.,-0.809016994374947,0.587785252292473));
#8936=DIRECTION('ref_axis',(-1.,0.,0.));
#8937=DIRECTION('center_axis',(1.,0.,0.));
#8938=DIRECTION('ref_axis',(0.,1.,0.));
#8939=DIRECTION('center_axis',(1.,0.,0.));
#8940=DIRECTION('ref_axis',(0.,0.,-1.));
#8941=DIRECTION('',(-0.53037253640964,0.847764691776206,1.03821231621387E-16));
#8942=DIRECTION('center_axis',(1.,0.,0.));
#8943=DIRECTION('ref_axis',(0.,0.,-1.));
#8944=DIRECTION('center_axis',(1.,0.,0.));
#8945=DIRECTION('ref_axis',(0.,0.,-1.));
#8946=DIRECTION('center_axis',(1.,0.,0.));
#8947=DIRECTION('ref_axis',(0.,0.,-1.));
#8948=DIRECTION('center_axis',(1.,0.,0.));
#8949=DIRECTION('ref_axis',(0.,0.,-1.));
#8950=DIRECTION('center_axis',(1.,0.,0.));
#8951=DIRECTION('ref_axis',(0.,0.,-1.));
#8952=DIRECTION('center_axis',(1.,0.,0.));
#8953=DIRECTION('ref_axis',(0.,0.,-1.));
#8954=DIRECTION('center_axis',(1.,0.,0.));
#8955=DIRECTION('ref_axis',(0.,0.,-1.));
#8956=DIRECTION('center_axis',(1.,0.,0.));
#8957=DIRECTION('ref_axis',(0.,0.,-1.));
#8958=DIRECTION('center_axis',(1.,0.,0.));
#8959=DIRECTION('ref_axis',(0.,0.,-1.));
#8960=DIRECTION('center_axis',(1.,0.,0.));
#8961=DIRECTION('ref_axis',(0.,0.,-1.));
#8962=DIRECTION('center_axis',(1.,0.,0.));
#8963=DIRECTION('ref_axis',(0.,0.,-1.));
#8964=DIRECTION('center_axis',(1.,0.,0.));
#8965=DIRECTION('ref_axis',(0.,0.,-1.));
#8966=DIRECTION('center_axis',(1.,0.,0.));
#8967=DIRECTION('ref_axis',(0.,1.,0.));
#8968=DIRECTION('center_axis',(1.,0.,0.));
#8969=DIRECTION('ref_axis',(0.,0.,-1.));
#8970=DIRECTION('center_axis',(1.,0.,0.));
#8971=DIRECTION('ref_axis',(0.,0.,-1.));
#8972=DIRECTION('center_axis',(1.,0.,0.));
#8973=DIRECTION('ref_axis',(0.,0.,-1.));
#8974=DIRECTION('center_axis',(1.,0.,0.));
#8975=DIRECTION('ref_axis',(0.,0.,-1.));
#8976=DIRECTION('',(-1.,0.,0.));
#8977=DIRECTION('center_axis',(1.,0.,0.));
#8978=DIRECTION('ref_axis',(0.,0.,-1.));
#8979=DIRECTION('center_axis',(1.,0.,0.));
#8980=DIRECTION('ref_axis',(0.,0.,-1.));
#8981=DIRECTION('center_axis',(1.,0.,0.));
#8982=DIRECTION('ref_axis',(0.,0.,-1.));
#8983=DIRECTION('center_axis',(1.,0.,0.));
#8984=DIRECTION('ref_axis',(0.,0.,-1.));
#8985=DIRECTION('center_axis',(1.,0.,0.));
#8986=DIRECTION('ref_axis',(0.,0.,-1.));
#8987=DIRECTION('center_axis',(1.,0.,0.));
#8988=DIRECTION('ref_axis',(0.,0.,-1.));
#8989=DIRECTION('center_axis',(1.,0.,0.));
#8990=DIRECTION('ref_axis',(0.,0.,-1.));
#8991=DIRECTION('center_axis',(1.,0.,0.));
#8992=DIRECTION('ref_axis',(0.,0.,-1.));
#8993=DIRECTION('center_axis',(1.,0.,0.));
#8994=DIRECTION('ref_axis',(0.,0.,-1.));
#8995=DIRECTION('center_axis',(0.,0.951056516295154,0.309016994374948));
#8996=DIRECTION('ref_axis',(1.,0.,0.));
#8997=DIRECTION('center_axis',(0.,-0.309016994374947,0.951056516295154));
#8998=DIRECTION('ref_axis',(-1.,0.,0.));
#8999=DIRECTION('center_axis',(1.,0.,0.));
#9000=DIRECTION('ref_axis',(0.,0.,-1.));
#9001=DIRECTION('center_axis',(1.,0.,0.));
#9002=DIRECTION('ref_axis',(0.,0.,-1.));
#9003=DIRECTION('center_axis',(1.,0.,0.));
#9004=DIRECTION('ref_axis',(0.,0.,-1.));
#9005=DIRECTION('center_axis',(1.,0.,0.));
#9006=DIRECTION('ref_axis',(0.,0.,-1.));
#9007=DIRECTION('center_axis',(0.,0.951056516295154,-0.309016994374948));
#9008=DIRECTION('ref_axis',(1.,0.,0.));
#9009=DIRECTION('center_axis',(0.,0.309016994374948,0.951056516295154));
#9010=DIRECTION('ref_axis',(-1.,0.,0.));
#9011=DIRECTION('center_axis',(1.,0.,0.));
#9012=DIRECTION('ref_axis',(0.,0.,-1.));
#9013=DIRECTION('center_axis',(1.,0.,0.));
#9014=DIRECTION('ref_axis',(0.,0.,-1.));
#9015=DIRECTION('center_axis',(1.,0.,0.));
#9016=DIRECTION('ref_axis',(0.,0.,-1.));
#9017=DIRECTION('center_axis',(1.,0.,0.));
#9018=DIRECTION('ref_axis',(0.,0.,-1.));
#9019=DIRECTION('center_axis',(0.,0.587785252292473,-0.809016994374947));
#9020=DIRECTION('ref_axis',(1.,0.,0.));
#9021=DIRECTION('center_axis',(0.,0.809016994374948,0.587785252292473));
#9022=DIRECTION('ref_axis',(-1.,0.,0.));
#9023=DIRECTION('center_axis',(1.,0.,0.));
#9024=DIRECTION('ref_axis',(0.,0.,-1.));
#9025=DIRECTION('center_axis',(1.,0.,0.));
#9026=DIRECTION('ref_axis',(0.,0.,-1.));
#9027=DIRECTION('center_axis',(1.,0.,0.));
#9028=DIRECTION('ref_axis',(0.,0.,-1.));
#9029=DIRECTION('center_axis',(1.,0.,0.));
#9030=DIRECTION('ref_axis',(0.,0.,-1.));
#9031=DIRECTION('center_axis',(0.,0.,-1.));
#9032=DIRECTION('ref_axis',(1.,0.,0.));
#9033=DIRECTION('center_axis',(0.,1.,-1.22464679914735E-16));
#9034=DIRECTION('ref_axis',(-1.,0.,0.));
#9035=DIRECTION('center_axis',(1.,0.,0.));
#9036=DIRECTION('ref_axis',(0.,0.,-1.));
#9037=DIRECTION('center_axis',(1.,0.,0.));
#9038=DIRECTION('ref_axis',(0.,0.,-1.));
#9039=DIRECTION('center_axis',(1.,0.,0.));
#9040=DIRECTION('ref_axis',(0.,0.,-1.));
#9041=DIRECTION('center_axis',(1.,0.,0.));
#9042=DIRECTION('ref_axis',(0.,0.,-1.));
#9043=DIRECTION('center_axis',(0.,-0.587785252292473,-0.809016994374948));
#9044=DIRECTION('ref_axis',(1.,0.,0.));
#9045=DIRECTION('center_axis',(0.,0.809016994374947,-0.587785252292473));
#9046=DIRECTION('ref_axis',(-1.,0.,0.));
#9047=DIRECTION('center_axis',(1.,0.,0.));
#9048=DIRECTION('ref_axis',(0.,0.,-1.));
#9049=DIRECTION('center_axis',(1.,0.,0.));
#9050=DIRECTION('ref_axis',(0.,0.,-1.));
#9051=DIRECTION('center_axis',(1.,0.,0.));
#9052=DIRECTION('ref_axis',(0.,0.,-1.));
#9053=DIRECTION('center_axis',(1.,0.,0.));
#9054=DIRECTION('ref_axis',(0.,0.,-1.));
#9055=DIRECTION('center_axis',(0.,-0.951056516295154,-0.309016994374948));
#9056=DIRECTION('ref_axis',(1.,0.,0.));
#9057=DIRECTION('center_axis',(0.,0.309016994374947,-0.951056516295154));
#9058=DIRECTION('ref_axis',(-1.,0.,0.));
#9059=DIRECTION('center_axis',(1.,0.,0.));
#9060=DIRECTION('ref_axis',(0.,-1.22464679914735E-16,1.));
#9061=DIRECTION('center_axis',(1.,0.,0.));
#9062=DIRECTION('ref_axis',(0.,0.,-1.));
#9063=DIRECTION('center_axis',(1.,0.,0.));
#9064=DIRECTION('ref_axis',(0.,-1.22464679914735E-16,1.));
#9065=DIRECTION('center_axis',(1.,0.,0.));
#9066=DIRECTION('ref_axis',(0.,0.,-1.));
#9067=DIRECTION('center_axis',(0.,-0.951056516295154,0.309016994374948));
#9068=DIRECTION('ref_axis',(1.,0.,0.));
#9069=DIRECTION('center_axis',(0.,-0.309016994374948,-0.951056516295154));
#9070=DIRECTION('ref_axis',(-1.,0.,0.));
#9071=DIRECTION('center_axis',(1.,0.,0.));
#9072=DIRECTION('ref_axis',(0.,0.,-1.));
#9073=DIRECTION('center_axis',(1.,0.,0.));
#9074=DIRECTION('ref_axis',(0.,0.,-1.));
#9075=DIRECTION('center_axis',(1.,0.,0.));
#9076=DIRECTION('ref_axis',(0.,0.,-1.));
#9077=DIRECTION('center_axis',(1.,0.,0.));
#9078=DIRECTION('ref_axis',(0.,0.,-1.));
#9079=DIRECTION('center_axis',(0.,-0.587785252292473,0.809016994374947));
#9080=DIRECTION('ref_axis',(1.,0.,0.));
#9081=DIRECTION('center_axis',(0.,-0.809016994374948,-0.587785252292473));
#9082=DIRECTION('ref_axis',(-1.,0.,0.));
#9083=DIRECTION('center_axis',(1.,0.,0.));
#9084=DIRECTION('ref_axis',(0.,1.,0.));
#9085=DIRECTION('center_axis',(1.,0.,0.));
#9086=DIRECTION('ref_axis',(0.,0.,-1.));
#9087=DIRECTION('center_axis',(1.,0.,0.));
#9088=DIRECTION('ref_axis',(0.,0.,-1.));
#9089=DIRECTION('',(-1.,0.,0.));
#9090=DIRECTION('center_axis',(1.,0.,0.));
#9091=DIRECTION('ref_axis',(0.,0.,-1.));
#9092=DIRECTION('center_axis',(1.,0.,0.));
#9093=DIRECTION('ref_axis',(0.,0.,-1.));
#9094=DIRECTION('center_axis',(1.,0.,0.));
#9095=DIRECTION('ref_axis',(0.,1.,0.));
#9096=DIRECTION('center_axis',(1.,0.,0.));
#9097=DIRECTION('ref_axis',(0.,0.,-1.));
#9098=DIRECTION('',(-1.,0.,0.));
#9099=DIRECTION('center_axis',(1.,0.,0.));
#9100=DIRECTION('ref_axis',(0.,0.,-1.));
#9101=DIRECTION('center_axis',(1.,0.,0.));
#9102=DIRECTION('ref_axis',(0.,0.,-1.));
#9103=DIRECTION('center_axis',(1.,0.,0.));
#9104=DIRECTION('ref_axis',(0.,0.,-1.));
#9105=DIRECTION('center_axis',(0.,0.,1.));
#9106=DIRECTION('ref_axis',(1.,0.,0.));
#9107=DIRECTION('center_axis',(0.,-1.,0.));
#9108=DIRECTION('ref_axis',(-1.,0.,0.));
#9109=DIRECTION('center_axis',(1.,0.,0.));
#9110=DIRECTION('ref_axis',(0.,0.,-1.));
#9111=DIRECTION('center_axis',(-1.,0.,0.));
#9112=DIRECTION('ref_axis',(0.,0.,1.));
#9113=DIRECTION('center_axis',(1.,0.,0.));
#9114=DIRECTION('ref_axis',(0.,0.,-1.));
#9115=DIRECTION('center_axis',(1.,0.,0.));
#9116=DIRECTION('ref_axis',(0.,1.,0.));
#9117=DIRECTION('center_axis',(1.,0.,0.));
#9118=DIRECTION('ref_axis',(0.,0.,-1.));
#9119=DIRECTION('',(-0.707106781186547,0.707106781186548,8.65956056235494E-17));
#9120=DIRECTION('center_axis',(1.,0.,0.));
#9121=DIRECTION('ref_axis',(0.,1.,0.));
#9122=DIRECTION('center_axis',(1.,0.,0.));
#9123=DIRECTION('ref_axis',(0.,0.,-1.));
#9124=DIRECTION('',(-1.,0.,0.));
#9125=DIRECTION('center_axis',(-1.,0.,0.));
#9126=DIRECTION('ref_axis',(0.,1.,0.));
#9127=DIRECTION('center_axis',(1.,0.,0.));
#9128=DIRECTION('ref_axis',(0.,0.,-1.));
#9129=DIRECTION('',(-0.707106781186548,-0.707106781186548,-8.65956056235493E-17));
#9130=DIRECTION('center_axis',(1.,0.,0.));
#9131=DIRECTION('ref_axis',(0.,0.,-1.));
#9132=DIRECTION('center_axis',(1.,0.,0.));
#9133=DIRECTION('ref_axis',(0.,0.,-1.));
#9134=DIRECTION('center_axis',(1.,0.,0.));
#9135=DIRECTION('ref_axis',(0.,1.,0.));
#9136=DIRECTION('',(-1.,0.,0.));
#9137=DIRECTION('center_axis',(1.,0.,0.));
#9138=DIRECTION('ref_axis',(0.,0.,-1.));
#9139=DIRECTION('center_axis',(1.,0.,0.));
#9140=DIRECTION('ref_axis',(0.,0.,-1.));
#9141=DIRECTION('center_axis',(1.,0.,0.));
#9142=DIRECTION('ref_axis',(0.,0.,-1.));
#9143=DIRECTION('center_axis',(1.,0.,0.));
#9144=DIRECTION('ref_axis',(0.,1.,0.));
#9145=DIRECTION('',(-0.707106781186548,0.707106781186548,8.65956056235493E-17));
#9146=DIRECTION('center_axis',(1.,0.,0.));
#9147=DIRECTION('ref_axis',(0.,0.,-1.));
#9148=DIRECTION('center_axis',(1.,0.,0.));
#9149=DIRECTION('ref_axis',(0.,1.,0.));
#9150=DIRECTION('',(-1.,0.,0.));
#9151=DIRECTION('center_axis',(1.,0.,0.));
#9152=DIRECTION('ref_axis',(0.,0.,-1.));
#9153=DIRECTION('center_axis',(-1.,0.,0.));
#9154=DIRECTION('ref_axis',(0.,1.,0.));
#9155=DIRECTION('',(-0.707106781186547,-0.707106781186548,-8.65956056235494E-17));
#9156=DIRECTION('center_axis',(1.,0.,0.));
#9157=DIRECTION('ref_axis',(0.,0.,-1.));
#9158=DIRECTION('center_axis',(-1.,0.,0.));
#9159=DIRECTION('ref_axis',(0.,0.,1.));
#9160=DIRECTION('axis',(0.,0.,1.));
#9161=DIRECTION('refdir',(1.,0.,0.));
#9162=DIRECTION('center_axis',(-1.,0.,0.));
#9163=DIRECTION('ref_axis',(0.,0.,1.));
#9164=DIRECTION('center_axis',(1.,0.,0.));
#9165=DIRECTION('ref_axis',(0.,0.,-1.));
#9166=DIRECTION('center_axis',(1.,0.,0.));
#9167=DIRECTION('ref_axis',(0.,0.,-1.));
#9168=DIRECTION('center_axis',(1.,0.,0.));
#9169=DIRECTION('ref_axis',(0.,1.,0.));
#9170=DIRECTION('center_axis',(1.,0.,0.));
#9171=DIRECTION('ref_axis',(0.,0.,-1.));
#9172=DIRECTION('',(-0.800000000000002,0.599999999999998,7.34788079488409E-17));
#9173=DIRECTION('center_axis',(-1.,0.,0.));
#9174=DIRECTION('ref_axis',(0.,0.,1.));
#9175=DIRECTION('center_axis',(1.,0.,0.));
#9176=DIRECTION('ref_axis',(0.,0.,-1.));
#9177=DIRECTION('center_axis',(-1.,0.,0.));
#9178=DIRECTION('ref_axis',(0.,1.,0.));
#9179=DIRECTION('',(-0.799999999999997,-0.600000000000003,-7.34788079488416E-17));
#9180=DIRECTION('center_axis',(1.,0.,0.));
#9181=DIRECTION('ref_axis',(0.,0.,-1.));
#9182=DIRECTION('center_axis',(-1.,0.,0.));
#9183=DIRECTION('ref_axis',(0.,0.,1.));
#9184=DIRECTION('center_axis',(1.,0.,0.));
#9185=DIRECTION('ref_axis',(0.,0.,-1.));
#9186=DIRECTION('center_axis',(1.,0.,0.));
#9187=DIRECTION('ref_axis',(0.,1.,0.));
#9188=DIRECTION('center_axis',(1.,0.,0.));
#9189=DIRECTION('ref_axis',(0.,0.,-1.));
#9190=DIRECTION('',(-0.707106781186547,0.707106781186548,8.65956056235494E-17));
#9191=DIRECTION('center_axis',(1.,0.,0.));
#9192=DIRECTION('ref_axis',(0.,1.,0.));
#9193=DIRECTION('center_axis',(1.,0.,0.));
#9194=DIRECTION('ref_axis',(0.,0.,-1.));
#9195=DIRECTION('',(-1.,0.,0.));
#9196=DIRECTION('center_axis',(-1.,0.,0.));
#9197=DIRECTION('ref_axis',(0.,1.,0.));
#9198=DIRECTION('center_axis',(1.,0.,0.));
#9199=DIRECTION('ref_axis',(0.,0.,-1.));
#9200=DIRECTION('',(-0.707106781186548,-0.707106781186548,-8.65956056235493E-17));
#9201=DIRECTION('center_axis',(1.,0.,0.));
#9202=DIRECTION('ref_axis',(0.,0.,-1.));
#9203=DIRECTION('center_axis',(1.,0.,0.));
#9204=DIRECTION('ref_axis',(0.,0.,-1.));
#9205=DIRECTION('center_axis',(1.,0.,0.));
#9206=DIRECTION('ref_axis',(0.,1.,0.));
#9207=DIRECTION('',(-0.799999999999998,0.600000000000003,7.34788079488415E-17));
#9208=DIRECTION('center_axis',(1.,0.,0.));
#9209=DIRECTION('ref_axis',(0.,0.,-1.));
#9210=DIRECTION('center_axis',(1.,0.,0.));
#9211=DIRECTION('ref_axis',(0.,0.,-1.));
#9212=DIRECTION('center_axis',(1.,0.,0.));
#9213=DIRECTION('ref_axis',(0.,0.,-1.));
#9214=DIRECTION('center_axis',(-1.,0.,0.));
#9215=DIRECTION('ref_axis',(0.,1.,0.));
#9216=DIRECTION('center_axis',(1.,0.,0.));
#9217=DIRECTION('ref_axis',(0.,0.,-1.));
#9218=DIRECTION('',(-0.800000000000002,-0.599999999999997,-7.34788079488409E-17));
#9219=DIRECTION('center_axis',(1.,0.,0.));
#9220=DIRECTION('ref_axis',(0.,0.,-1.));
#9221=DIRECTION('center_axis',(1.,0.,0.));
#9222=DIRECTION('ref_axis',(0.,0.,-1.));
#9223=DIRECTION('center_axis',(1.,0.,0.));
#9224=DIRECTION('ref_axis',(0.,1.,0.));
#9225=DIRECTION('',(-0.707106781186548,0.707106781186548,8.65956056235493E-17));
#9226=DIRECTION('center_axis',(1.,0.,0.));
#9227=DIRECTION('ref_axis',(0.,0.,-1.));
#9228=DIRECTION('center_axis',(1.,0.,0.));
#9229=DIRECTION('ref_axis',(0.,1.,0.));
#9230=DIRECTION('',(-1.,0.,0.));
#9231=DIRECTION('center_axis',(1.,0.,0.));
#9232=DIRECTION('ref_axis',(0.,0.,-1.));
#9233=DIRECTION('center_axis',(-1.,0.,0.));
#9234=DIRECTION('ref_axis',(0.,1.,0.));
#9235=DIRECTION('',(-0.707106781186547,-0.707106781186548,-8.65956056235494E-17));
#9236=DIRECTION('axis',(0.,0.,1.));
#9237=DIRECTION('refdir',(1.,0.,0.));
#9238=DIRECTION('center_axis',(1.,0.,0.));
#9239=DIRECTION('ref_axis',(0.,1.,0.));
#9240=DIRECTION('center_axis',(1.,0.,0.));
#9241=DIRECTION('ref_axis',(0.,0.,-1.));
#9242=DIRECTION('',(-1.,0.,0.));
#9243=DIRECTION('center_axis',(1.,0.,0.));
#9244=DIRECTION('ref_axis',(0.,0.,-1.));
#9245=DIRECTION('center_axis',(1.,0.,0.));
#9246=DIRECTION('ref_axis',(0.,0.,-1.));
#9247=DIRECTION('center_axis',(1.,0.,0.));
#9248=DIRECTION('ref_axis',(0.,0.,-1.));
#9249=DIRECTION('center_axis',(1.,0.,0.));
#9250=DIRECTION('ref_axis',(0.,1.,0.));
#9251=DIRECTION('',(-1.,0.,0.));
#9252=DIRECTION('center_axis',(1.,0.,0.));
#9253=DIRECTION('ref_axis',(0.,0.,-1.));
#9254=DIRECTION('center_axis',(-1.,0.,0.));
#9255=DIRECTION('ref_axis',(0.,0.,1.));
#9256=DIRECTION('axis',(0.,0.,1.));
#9257=DIRECTION('refdir',(1.,0.,0.));
#9258=DIRECTION('center_axis',(1.,0.,0.));
#9259=DIRECTION('ref_axis',(0.,1.,0.));
#9260=DIRECTION('',(-1.,0.,0.));
#9261=DIRECTION('center_axis',(1.,0.,0.));
#9262=DIRECTION('ref_axis',(0.,1.,0.));
#9263=DIRECTION('center_axis',(1.,0.,0.));
#9264=DIRECTION('ref_axis',(0.,1.,0.));
#9265=DIRECTION('',(-1.,0.,0.));
#9266=DIRECTION('center_axis',(1.,0.,0.));
#9267=DIRECTION('ref_axis',(0.,1.,0.));
#9268=DIRECTION('',(-1.,0.,0.));
#9269=DIRECTION('center_axis',(1.,0.,0.));
#9270=DIRECTION('ref_axis',(0.,1.,0.));
#9271=DIRECTION('',(-1.,0.,0.));
#9272=DIRECTION('center_axis',(1.,0.,0.));
#9273=DIRECTION('ref_axis',(0.,1.,0.));
#9274=DIRECTION('',(-1.,0.,0.));
#9275=DIRECTION('center_axis',(1.,0.,0.));
#9276=DIRECTION('ref_axis',(0.,1.,4.77055255383026E-15));
#9277=DIRECTION('',(1.,0.,0.));
#9278=DIRECTION('center_axis',(1.,0.,0.));
#9279=DIRECTION('ref_axis',(0.,1.,4.77055255383026E-15));
#9280=DIRECTION('center_axis',(1.,0.,0.));
#9281=DIRECTION('ref_axis',(0.,1.,4.77055255383026E-15));
#9282=DIRECTION('',(1.,0.,0.));
#9283=DIRECTION('center_axis',(1.,0.,0.));
#9284=DIRECTION('ref_axis',(0.,1.,4.77055255383026E-15));
#9285=DIRECTION('',(1.,0.,0.));
#9286=DIRECTION('center_axis',(1.,0.,0.));
#9287=DIRECTION('ref_axis',(0.,1.,4.77055255383026E-15));
#9288=DIRECTION('',(1.,0.,0.));
#9289=DIRECTION('center_axis',(1.,0.,0.));
#9290=DIRECTION('ref_axis',(0.,0.,-1.));
#9291=DIRECTION('center_axis',(-1.,0.,0.));
#9292=DIRECTION('ref_axis',(0.,1.,0.));
#9293=DIRECTION('center_axis',(-1.,0.,0.));
#9294=DIRECTION('ref_axis',(0.,1.,0.));
#9295=DIRECTION('center_axis',(1.,0.,0.));
#9296=DIRECTION('ref_axis',(0.,0.,-1.));
#9297=DIRECTION('center_axis',(1.,0.,0.));
#9298=DIRECTION('ref_axis',(0.,1.,0.));
#9299=DIRECTION('center_axis',(1.,0.,0.));
#9300=DIRECTION('ref_axis',(0.,1.,0.));
#9301=DIRECTION('center_axis',(-1.,0.,0.));
#9302=DIRECTION('ref_axis',(0.,1.,4.77055255383026E-15));
#9303=DIRECTION('center_axis',(1.,0.,0.));
#9304=DIRECTION('ref_axis',(0.,0.889087843978286,0.457736611699396));
#9305=DIRECTION('center_axis',(1.,0.,0.));
#9306=DIRECTION('ref_axis',(0.,1.,0.));
#9307=DIRECTION('',(0.520759202022183,-0.853703609872431,-1.04548539325081E-16));
#9308=DIRECTION('center_axis',(-1.,0.,0.));
#9309=DIRECTION('ref_axis',(0.,1.,0.));
#9310=DIRECTION('center_axis',(0.,-0.5,0.866025403784439));
#9311=DIRECTION('ref_axis',(0.,-0.866025403784439,-0.5));
#9312=DIRECTION('',(0.,0.866025403784439,0.5));
#9313=DIRECTION('',(1.,0.,0.));
#9314=DIRECTION('',(0.,-0.866025403784439,-0.5));
#9315=DIRECTION('',(1.,0.,0.));
#9316=DIRECTION('center_axis',(0.,0.5,0.866025403784439));
#9317=DIRECTION('ref_axis',(0.,-0.866025403784439,0.5));
#9318=DIRECTION('',(0.,0.866025403784439,-0.5));
#9319=DIRECTION('',(0.,-0.866025403784439,0.5));
#9320=DIRECTION('',(1.,0.,0.));
#9321=DIRECTION('center_axis',(0.,1.,-3.60555503696918E-16));
#9322=DIRECTION('ref_axis',(0.,3.60555503696918E-16,1.));
#9323=DIRECTION('',(0.,-3.60555503696918E-16,-1.));
#9324=DIRECTION('',(0.,3.60555503696918E-16,1.));
#9325=DIRECTION('',(1.,0.,0.));
#9326=DIRECTION('center_axis',(0.,0.5,-0.866025403784439));
#9327=DIRECTION('ref_axis',(0.,0.866025403784439,0.5));
#9328=DIRECTION('',(0.,-0.866025403784439,-0.5));
#9329=DIRECTION('',(0.,0.866025403784439,0.5));
#9330=DIRECTION('',(1.,0.,0.));
#9331=DIRECTION('center_axis',(0.,-0.5,-0.866025403784439));
#9332=DIRECTION('ref_axis',(0.,0.866025403784439,-0.5));
#9333=DIRECTION('',(0.,-0.866025403784439,0.5));
#9334=DIRECTION('',(0.,0.866025403784439,-0.5));
#9335=DIRECTION('',(1.,0.,0.));
#9336=DIRECTION('center_axis',(0.,-1.,-1.20185167898973E-16));
#9337=DIRECTION('ref_axis',(0.,1.20185167898973E-16,-1.));
#9338=DIRECTION('',(0.,-1.20185167898973E-16,1.));
#9339=DIRECTION('',(0.,1.20185167898973E-16,-1.));
#9340=DIRECTION('center_axis',(1.,0.,0.));
#9341=DIRECTION('ref_axis',(0.,0.,-1.));
#9342=DIRECTION('center_axis',(-1.,0.,0.));
#9343=DIRECTION('ref_axis',(0.,0.,1.));
#9344=DIRECTION('center_axis',(1.,0.,0.));
#9345=DIRECTION('ref_axis',(0.,0.,-1.));
#9346=DIRECTION('center_axis',(1.,0.,0.));
#9347=DIRECTION('ref_axis',(0.,1.,0.));
#9348=DIRECTION('',(-0.66896473162245,0.743294146247166,9.10272797026557E-17));
#9349=DIRECTION('center_axis',(1.,0.,0.));
#9350=DIRECTION('ref_axis',(0.,-0.163995302605342,-0.986461119722101));
#9351=DIRECTION('center_axis',(-1.,0.,0.));
#9352=DIRECTION('ref_axis',(0.,1.,0.));
#9353=DIRECTION('center_axis',(-1.,0.,0.));
#9354=DIRECTION('ref_axis',(0.,1.,0.));
#9355=DIRECTION('center_axis',(1.,0.,0.));
#9356=DIRECTION('ref_axis',(0.,0.,-1.));
#9357=DIRECTION('',(-0.707106781186548,-0.707106781186547,-8.65956056235493E-17));
#9358=DIRECTION('center_axis',(1.,0.,0.));
#9359=DIRECTION('ref_axis',(0.,0.,-1.));
#9360=DIRECTION('axis',(0.,0.,1.));
#9361=DIRECTION('refdir',(1.,0.,0.));
#9362=DIRECTION('center_axis',(1.,0.,0.));
#9363=DIRECTION('ref_axis',(0.,0.,-1.));
#9364=DIRECTION('center_axis',(1.,0.,0.));
#9365=DIRECTION('ref_axis',(0.,0.,-1.));
#9366=DIRECTION('',(1.,0.,0.));
#9367=DIRECTION('center_axis',(-1.,0.,0.));
#9368=DIRECTION('ref_axis',(0.,0.,-1.));
#9369=DIRECTION('center_axis',(1.,0.,0.));
#9370=DIRECTION('ref_axis',(0.,0.,-1.));
#9371=DIRECTION('center_axis',(1.,0.,0.));
#9372=DIRECTION('ref_axis',(0.,0.,-1.));
#9373=DIRECTION('',(1.,0.,0.));
#9374=DIRECTION('center_axis',(-1.,0.,0.));
#9375=DIRECTION('ref_axis',(0.,0.,-1.));
#9376=DIRECTION('center_axis',(1.,0.,0.));
#9377=DIRECTION('ref_axis',(0.,-1.,1.22464679914735E-16));
#9378=DIRECTION('',(-1.,0.,0.));
#9379=DIRECTION('center_axis',(1.,0.,0.));
#9380=DIRECTION('ref_axis',(0.,0.,-1.));
#9381=DIRECTION('',(1.,0.,0.));
#9382=DIRECTION('center_axis',(1.,0.,0.));
#9383=DIRECTION('ref_axis',(0.,0.,-1.));
#9384=DIRECTION('center_axis',(-1.,0.,0.));
#9385=DIRECTION('ref_axis',(0.,0.,1.));
#9386=DIRECTION('',(0.,1.,0.));
#9387=DIRECTION('',(0.,0.,-1.));
#9388=DIRECTION('',(0.,-1.,0.));
#9389=DIRECTION('center_axis',(1.,0.,0.));
#9390=DIRECTION('ref_axis',(0.,0.,-1.));
#9391=DIRECTION('',(0.,-1.,0.));
#9392=DIRECTION('',(0.,0.,1.));
#9393=DIRECTION('',(0.,1.,0.));
#9394=DIRECTION('center_axis',(0.,0.,-1.));
#9395=DIRECTION('ref_axis',(0.,1.,0.));
#9396=DIRECTION('',(-1.,0.,0.));
#9397=DIRECTION('',(0.,1.,0.));
#9398=DIRECTION('',(1.,0.,0.));
#9399=DIRECTION('center_axis',(0.,-1.,0.));
#9400=DIRECTION('ref_axis',(0.,0.,-1.));
#9401=DIRECTION('',(0.,0.,-1.));
#9402=DIRECTION('',(1.,0.,0.));
#9403=DIRECTION('center_axis',(0.,0.,1.));
#9404=DIRECTION('ref_axis',(0.,-1.,0.));
#9405=DIRECTION('',(0.,-1.,0.));
#9406=DIRECTION('center_axis',(0.,0.,-1.));
#9407=DIRECTION('ref_axis',(0.,1.,0.));
#9408=DIRECTION('',(0.,1.,0.));
#9409=DIRECTION('',(1.,0.,0.));
#9410=DIRECTION('center_axis',(0.,0.,1.));
#9411=DIRECTION('ref_axis',(0.,-1.,0.));
#9412=DIRECTION('',(1.,0.,0.));
#9413=DIRECTION('',(1.,0.,0.));
#9414=DIRECTION('',(0.,-1.,0.));
#9415=DIRECTION('center_axis',(0.,-1.,0.));
#9416=DIRECTION('ref_axis',(0.,0.,-1.));
#9417=DIRECTION('',(0.,0.,-1.));
#9418=DIRECTION('center_axis',(1.,0.,0.));
#9419=DIRECTION('ref_axis',(0.,0.,-1.));
#9420=DIRECTION('center_axis',(1.,0.,0.));
#9421=DIRECTION('ref_axis',(0.,0.,-1.));
#9422=DIRECTION('center_axis',(1.,0.,0.));
#9423=DIRECTION('ref_axis',(0.,-1.,-1.22464679914735E-16));
#9424=DIRECTION('',(0.,0.,1.));
#9425=DIRECTION('',(1.,0.,0.));
#9426=DIRECTION('',(0.,0.,-1.));
#9427=DIRECTION('',(0.,1.,0.));
#9428=DIRECTION('',(0.,0.,1.));
#9429=DIRECTION('',(1.,0.,0.));
#9430=DIRECTION('',(5.55111512312578E-17,0.,-1.));
#9431=DIRECTION('',(0.,1.,0.));
#9432=DIRECTION('',(0.,-5.55111512312578E-17,1.));
#9433=DIRECTION('',(1.,0.,0.));
#9434=DIRECTION('',(0.,0.,-1.));
#9435=DIRECTION('',(0.,1.,0.));
#9436=DIRECTION('',(0.,0.,1.));
#9437=DIRECTION('',(0.,-1.,0.));
#9438=DIRECTION('',(0.,0.,1.));
#9439=DIRECTION('',(1.,0.,0.));
#9440=DIRECTION('',(0.,0.,1.));
#9441=DIRECTION('',(-1.,0.,0.));
#9442=DIRECTION('',(0.,-5.55111512312578E-17,1.));
#9443=DIRECTION('',(1.,0.,0.));
#9444=DIRECTION('',(5.55111512312578E-17,0.,-1.));
#9445=DIRECTION('',(0.,1.,0.));
#9446=DIRECTION('',(-1.,0.,0.));
#9447=DIRECTION('',(0.,-5.55111512312578E-17,1.));
#9448=DIRECTION('',(-1.,0.,0.));
#9449=DIRECTION('',(0.,-1.,-5.55111512312578E-17));
#9450=DIRECTION('',(0.,-1.,0.));
#9451=DIRECTION('',(5.55111512312578E-17,0.,-1.));
#9452=DIRECTION('',(0.,-1.,0.));
#9453=DIRECTION('',(-1.,0.,-5.55111512312578E-17));
#9454=DIRECTION('',(0.,0.,1.));
#9455=DIRECTION('',(1.,0.,0.));
#9456=DIRECTION('',(0.,0.,1.));
#9457=DIRECTION('',(-1.,0.,0.));
#9458=DIRECTION('',(0.,0.,-1.));
#9459=DIRECTION('',(0.,1.,0.));
#9460=CARTESIAN_POINT('',(0.,0.,0.));
#9461=CARTESIAN_POINT('',(0.,0.,0.));
#9462=CARTESIAN_POINT('Origin',(0.,54.15,55.));
#9463=CARTESIAN_POINT('',(-14.,54.,55.));
#9464=CARTESIAN_POINT('Origin',(0.,54.,55.));
#9465=CARTESIAN_POINT('',(-14.,53.3,55.));
#9466=CARTESIAN_POINT('',(-14.,54.15,55.));
#9467=CARTESIAN_POINT('Origin',(0.,53.3,55.));
#9468=CARTESIAN_POINT('Origin',(14.7,53.3,55.));
#9469=CARTESIAN_POINT('',(-14.7,53.3,55.));
#9470=CARTESIAN_POINT('Origin',(0.,53.3,55.));
#9471=CARTESIAN_POINT('Origin',(0.,52.65,55.));
#9472=CARTESIAN_POINT('',(-14.7,52.,55.));
#9473=CARTESIAN_POINT('',(-14.7,52.65,55.));
#9474=CARTESIAN_POINT('Origin',(0.,52.,55.));
#9475=CARTESIAN_POINT('Origin',(14.,52.,55.));
#9476=CARTESIAN_POINT('',(-14.,52.,55.));
#9477=CARTESIAN_POINT('Origin',(0.,52.,55.));
#9478=CARTESIAN_POINT('Origin',(0.,48.,55.));
#9479=CARTESIAN_POINT('',(-14.,44.,55.));
#9480=CARTESIAN_POINT('',(-14.,48.,55.));
#9481=CARTESIAN_POINT('Origin',(0.,44.,55.));
#9482=CARTESIAN_POINT('Origin',(12.,44.,55.));
#9483=CARTESIAN_POINT('',(-12.,44.,55.));
#9484=CARTESIAN_POINT('Origin',(0.,44.,55.));
#9485=CARTESIAN_POINT('Origin',(0.,41.,55.));
#9486=CARTESIAN_POINT('',(-12.,38.,55.));
#9487=CARTESIAN_POINT('',(-12.,41.,55.));
#9488=CARTESIAN_POINT('Origin',(0.,38.,55.));
#9489=CARTESIAN_POINT('Origin',(14.,38.,55.));
#9490=CARTESIAN_POINT('',(-14.,38.,55.));
#9491=CARTESIAN_POINT('Origin',(0.,38.,55.));
#9492=CARTESIAN_POINT('Origin',(0.,32.5,55.));
#9493=CARTESIAN_POINT('',(-14.,28.,55.));
#9494=CARTESIAN_POINT('',(-14.,32.5,55.));
#9495=CARTESIAN_POINT('Origin',(0.,28.,55.));
#9496=CARTESIAN_POINT('Origin',(-40.15,0.,55.));
#9497=CARTESIAN_POINT('',(-40.,-14.,55.));
#9498=CARTESIAN_POINT('Origin',(-40.,0.,55.));
#9499=CARTESIAN_POINT('',(-39.3,-14.,55.));
#9500=CARTESIAN_POINT('',(-40.15,-14.,55.));
#9501=CARTESIAN_POINT('Origin',(-39.3,0.,55.));
#9502=CARTESIAN_POINT('Origin',(-39.3,14.7,55.));
#9503=CARTESIAN_POINT('',(-39.3,-14.7,55.));
#9504=CARTESIAN_POINT('Origin',(-39.3,0.,55.));
#9505=CARTESIAN_POINT('Origin',(-38.65,0.,55.));
#9506=CARTESIAN_POINT('',(-38.,-14.7,55.));
#9507=CARTESIAN_POINT('',(-38.65,-14.7,55.));
#9508=CARTESIAN_POINT('Origin',(-38.,0.,55.));
#9509=CARTESIAN_POINT('Origin',(-38.,14.,55.));
#9510=CARTESIAN_POINT('',(-38.,-14.,55.));
#9511=CARTESIAN_POINT('Origin',(-38.,0.,55.));
#9512=CARTESIAN_POINT('Origin',(-34.,0.,55.));
#9513=CARTESIAN_POINT('',(-30.,-14.,55.));
#9514=CARTESIAN_POINT('',(-34.,-14.,55.));
#9515=CARTESIAN_POINT('Origin',(-30.,0.,55.));
#9516=CARTESIAN_POINT('Origin',(-30.,12.,55.));
#9517=CARTESIAN_POINT('',(-30.,-12.,55.));
#9518=CARTESIAN_POINT('Origin',(-30.,0.,55.));
#9519=CARTESIAN_POINT('Origin',(-28.5,0.,55.));
#9520=CARTESIAN_POINT('',(-28.,-12.,55.));
#9521=CARTESIAN_POINT('',(-28.5,-12.,55.));
#9522=CARTESIAN_POINT('Origin',(-28.,0.,55.));
#9523=CARTESIAN_POINT('Origin',(28.5,0.,55.));
#9524=CARTESIAN_POINT('',(28.,-12.,55.));
#9525=CARTESIAN_POINT('Origin',(28.,0.,55.));
#9526=CARTESIAN_POINT('',(30.,-12.,55.));
#9527=CARTESIAN_POINT('',(28.5,-12.,55.));
#9528=CARTESIAN_POINT('Origin',(30.,0.,55.));
#9529=CARTESIAN_POINT('Origin',(30.,14.,55.));
#9530=CARTESIAN_POINT('',(30.,-14.,55.));
#9531=CARTESIAN_POINT('Origin',(30.,0.,55.));
#9532=CARTESIAN_POINT('Origin',(34.,0.,55.));
#9533=CARTESIAN_POINT('',(38.,-14.,55.));
#9534=CARTESIAN_POINT('',(34.,-14.,55.));
#9535=CARTESIAN_POINT('Origin',(38.,0.,55.));
#9536=CARTESIAN_POINT('Origin',(38.,14.7,55.));
#9537=CARTESIAN_POINT('',(38.,-14.7,55.));
#9538=CARTESIAN_POINT('Origin',(38.,0.,55.));
#9539=CARTESIAN_POINT('Origin',(38.65,0.,55.));
#9540=CARTESIAN_POINT('',(39.3,-14.7,55.));
#9541=CARTESIAN_POINT('',(38.65,-14.7,55.));
#9542=CARTESIAN_POINT('Origin',(39.3,0.,55.));
#9543=CARTESIAN_POINT('Origin',(39.3,14.,55.));
#9544=CARTESIAN_POINT('',(39.3,-14.,55.));
#9545=CARTESIAN_POINT('Origin',(39.3,0.,55.));
#9546=CARTESIAN_POINT('Origin',(40.15,0.,55.));
#9547=CARTESIAN_POINT('',(40.,-14.,55.));
#9548=CARTESIAN_POINT('',(40.15,-14.,55.));
#9549=CARTESIAN_POINT('Origin',(40.,0.,55.));
#9550=CARTESIAN_POINT('Origin',(0.,41.5,55.));
#9551=CARTESIAN_POINT('',(-20.,41.5,55.));
#9552=CARTESIAN_POINT('',(-2.44929359829471E-15,41.5,75.));
#9553=CARTESIAN_POINT('Origin',(0.,41.5,55.));
#9554=CARTESIAN_POINT('',(-2.63299061816681E-15,40.,76.5));
#9555=CARTESIAN_POINT('Origin',(-2.63299061816681E-15,41.5,76.5));
#9556=CARTESIAN_POINT('Origin',(0.,40.,55.));
#9557=CARTESIAN_POINT('Origin',(0.,41.5,55.));
#9558=CARTESIAN_POINT('Origin',(0.,46.75,55.));
#9559=CARTESIAN_POINT('',(-20.,53.,55.));
#9560=CARTESIAN_POINT('',(-20.,46.75,55.));
#9561=CARTESIAN_POINT('',(20.,53.,55.));
#9562=CARTESIAN_POINT('Origin',(0.,53.,55.));
#9563=CARTESIAN_POINT('Origin',(0.,53.,55.));
#9564=CARTESIAN_POINT('Origin',(40.,40.,15.));
#9565=CARTESIAN_POINT('',(-38.,40.,15.8));
#9566=CARTESIAN_POINT('',(38.,40.,15.8));
#9567=CARTESIAN_POINT('',(20.,40.,15.8));
#9568=CARTESIAN_POINT('',(-39.2,40.,17.));
#9569=CARTESIAN_POINT('Origin',(-38.,40.,17.));
#9570=CARTESIAN_POINT('',(-39.2,40.,93.));
#9571=CARTESIAN_POINT('',(-39.2,40.,15.));
#9572=CARTESIAN_POINT('',(-38.,40.,94.2));
#9573=CARTESIAN_POINT('Origin',(-38.,40.,93.));
#9574=CARTESIAN_POINT('',(38.,40.,94.2));
#9575=CARTESIAN_POINT('',(20.,40.,94.2));
#9576=CARTESIAN_POINT('',(39.2,40.,93.));
#9577=CARTESIAN_POINT('Origin',(38.,40.,93.));
#9578=CARTESIAN_POINT('',(39.2,40.,17.));
#9579=CARTESIAN_POINT('',(39.2,40.,15.));
#9580=CARTESIAN_POINT('Origin',(38.,40.,17.));
#9581=CARTESIAN_POINT('Origin',(0.,53.5,55.));
#9582=CARTESIAN_POINT('',(19.,54.,55.));
#9583=CARTESIAN_POINT('',(19.5,53.5,55.));
#9584=CARTESIAN_POINT('Origin',(0.,54.,55.));
#9585=CARTESIAN_POINT('Origin',(20.,54.,55.));
#9586=CARTESIAN_POINT('Origin',(20.,39.6,15.4));
#9587=CARTESIAN_POINT('',(-38.,39.2,15.));
#9588=CARTESIAN_POINT('',(-38.,39.2,15.));
#9589=CARTESIAN_POINT('',(38.,39.2,15.));
#9590=CARTESIAN_POINT('',(38.,40.,15.8));
#9591=CARTESIAN_POINT('',(20.,39.2,15.));
#9592=CARTESIAN_POINT('Origin',(-38.,39.6,17.));
#9593=CARTESIAN_POINT('',(-40.,39.2,17.));
#9594=CARTESIAN_POINT('Origin',(-38.,39.2,17.));
#9595=CARTESIAN_POINT('',(-40.,39.2,17.));
#9596=CARTESIAN_POINT('Origin',(-39.6,39.6,15.));
#9597=CARTESIAN_POINT('',(-40.,39.2,93.));
#9598=CARTESIAN_POINT('',(-40.,39.2,93.));
#9599=CARTESIAN_POINT('',(-40.,39.2,15.));
#9600=CARTESIAN_POINT('Origin',(-38.,39.6,93.));
#9601=CARTESIAN_POINT('',(-38.,39.2,95.));
#9602=CARTESIAN_POINT('Origin',(-38.,39.2,93.));
#9603=CARTESIAN_POINT('',(-38.,39.2,95.));
#9604=CARTESIAN_POINT('Origin',(20.,39.6,94.6));
#9605=CARTESIAN_POINT('',(38.,39.2,95.));
#9606=CARTESIAN_POINT('',(20.,39.2,95.));
#9607=CARTESIAN_POINT('',(38.,39.2,95.));
#9608=CARTESIAN_POINT('Origin',(38.,39.6,93.));
#9609=CARTESIAN_POINT('',(40.,39.2,93.));
#9610=CARTESIAN_POINT('Origin',(38.,39.2,93.));
#9611=CARTESIAN_POINT('',(40.,39.2,93.));
#9612=CARTESIAN_POINT('Origin',(39.6,39.6,15.));
#9613=CARTESIAN_POINT('',(40.,39.2,17.));
#9614=CARTESIAN_POINT('',(40.,39.2,15.));
#9615=CARTESIAN_POINT('',(40.,39.2,17.));
#9616=CARTESIAN_POINT('Origin',(38.,39.6,17.));
#9617=CARTESIAN_POINT('Origin',(38.,39.2,17.));
#9618=CARTESIAN_POINT('Origin',(-38.,25.,93.));
#9619=CARTESIAN_POINT('',(-40.,-19.,93.));
#9620=CARTESIAN_POINT('',(-40.,25.,93.));
#9621=CARTESIAN_POINT('',(-38.,-19.,95.));
#9622=CARTESIAN_POINT('Origin',(-38.,-19.,93.));
#9623=CARTESIAN_POINT('',(-38.,25.,95.));
#9624=CARTESIAN_POINT('Origin',(-40.,40.,15.));
#9625=CARTESIAN_POINT('',(-40.,-19.,17.));
#9626=CARTESIAN_POINT('',(-40.,25.,17.));
#9627=CARTESIAN_POINT('',(-40.,-19.,15.));
#9628=CARTESIAN_POINT('Origin',(-38.,25.,17.));
#9629=CARTESIAN_POINT('',(-38.,-19.,15.));
#9630=CARTESIAN_POINT('',(-38.,25.,15.));
#9631=CARTESIAN_POINT('Origin',(-38.,-19.,17.));
#9632=CARTESIAN_POINT('Origin',(0.,10.,15.));
#9633=CARTESIAN_POINT('',(38.,-19.,15.));
#9634=CARTESIAN_POINT('',(38.,-5.,15.));
#9635=CARTESIAN_POINT('',(-20.,-19.,15.));
#9636=CARTESIAN_POINT('Origin',(-38.,-19.5,93.));
#9637=CARTESIAN_POINT('',(-38.,-20.,94.));
#9638=CARTESIAN_POINT('',(-38.,-20.,94.));
#9639=CARTESIAN_POINT('',(-39.,-20.,93.));
#9640=CARTESIAN_POINT('',(-40.,-19.,93.));
#9641=CARTESIAN_POINT('Origin',(-38.,-20.,93.));
#9642=CARTESIAN_POINT('Origin',(-20.,-19.5,94.5));
#9643=CARTESIAN_POINT('',(38.,-20.,94.));
#9644=CARTESIAN_POINT('',(38.,-19.,95.));
#9645=CARTESIAN_POINT('',(38.,-20.,94.));
#9646=CARTESIAN_POINT('',(-20.,-19.,95.));
#9647=CARTESIAN_POINT('',(-20.,-20.,94.));
#9648=CARTESIAN_POINT('Origin',(38.,-19.5,93.));
#9649=CARTESIAN_POINT('',(39.,-20.,93.));
#9650=CARTESIAN_POINT('',(40.,-19.,93.));
#9651=CARTESIAN_POINT('',(39.,-20.,93.));
#9652=CARTESIAN_POINT('Origin',(38.,-19.,93.));
#9653=CARTESIAN_POINT('Origin',(38.,-20.,93.));
#9654=CARTESIAN_POINT('Origin',(39.5,-19.5,15.));
#9655=CARTESIAN_POINT('',(39.,-20.,17.));
#9656=CARTESIAN_POINT('',(39.,-20.,15.));
#9657=CARTESIAN_POINT('',(40.,-19.,17.));
#9658=CARTESIAN_POINT('',(39.,-20.,17.));
#9659=CARTESIAN_POINT('',(40.,-19.,15.));
#9660=CARTESIAN_POINT('Origin',(38.,-19.5,17.));
#9661=CARTESIAN_POINT('',(38.,-20.,16.));
#9662=CARTESIAN_POINT('',(38.,-20.,16.));
#9663=CARTESIAN_POINT('Origin',(38.,-19.,17.));
#9664=CARTESIAN_POINT('Origin',(38.,-20.,17.));
#9665=CARTESIAN_POINT('Origin',(-20.,-19.5,15.5));
#9666=CARTESIAN_POINT('',(-38.,-20.,16.));
#9667=CARTESIAN_POINT('',(-20.,-20.,16.));
#9668=CARTESIAN_POINT('',(-38.,-20.,16.));
#9669=CARTESIAN_POINT('Origin',(-38.,-19.5,17.));
#9670=CARTESIAN_POINT('',(-39.,-20.,17.));
#9671=CARTESIAN_POINT('',(-39.,-20.,17.));
#9672=CARTESIAN_POINT('Origin',(-38.,-20.,17.));
#9673=CARTESIAN_POINT('Origin',(-39.5,-19.5,15.));
#9674=CARTESIAN_POINT('',(-39.,-20.,15.));
#9675=CARTESIAN_POINT('Origin',(-40.,-20.,15.));
#9676=CARTESIAN_POINT('',(-25.,-20.,84.));
#9677=CARTESIAN_POINT('',(-29.,-20.,80.));
#9678=CARTESIAN_POINT('Origin',(-25.,-20.,80.));
#9679=CARTESIAN_POINT('',(25.,-20.,84.));
#9680=CARTESIAN_POINT('',(-20.,-20.,84.));
#9681=CARTESIAN_POINT('',(29.,-20.,80.));
#9682=CARTESIAN_POINT('Origin',(25.,-20.,80.));
#9683=CARTESIAN_POINT('',(29.,-20.,30.));
#9684=CARTESIAN_POINT('',(29.,-20.,21.));
#9685=CARTESIAN_POINT('',(25.,-20.,26.));
#9686=CARTESIAN_POINT('Origin',(25.,-20.,30.));
#9687=CARTESIAN_POINT('',(-25.,-20.,26.));
#9688=CARTESIAN_POINT('',(-20.,-20.,26.));
#9689=CARTESIAN_POINT('',(-29.,-20.,30.));
#9690=CARTESIAN_POINT('Origin',(-25.,-20.,30.));
#9691=CARTESIAN_POINT('',(-29.,-20.,21.));
#9692=CARTESIAN_POINT('Origin',(-25.,-19.5,80.));
#9693=CARTESIAN_POINT('',(-28.,-19.,80.));
#9694=CARTESIAN_POINT('',(-29.,-20.,80.));
#9695=CARTESIAN_POINT('',(-25.,-19.,83.));
#9696=CARTESIAN_POINT('Origin',(-25.,-19.,80.));
#9697=CARTESIAN_POINT('',(-25.,-19.,83.));
#9698=CARTESIAN_POINT('Origin',(-28.5,-19.5,21.));
#9699=CARTESIAN_POINT('',(-28.,-19.,30.));
#9700=CARTESIAN_POINT('',(-29.,-20.,30.));
#9701=CARTESIAN_POINT('',(-28.,-19.,21.));
#9702=CARTESIAN_POINT('Origin',(-25.,-19.5,30.));
#9703=CARTESIAN_POINT('',(-25.,-19.,27.));
#9704=CARTESIAN_POINT('',(-25.,-20.,26.));
#9705=CARTESIAN_POINT('Origin',(-25.,-19.,30.));
#9706=CARTESIAN_POINT('Origin',(-20.,-19.5,26.5));
#9707=CARTESIAN_POINT('',(25.,-19.,27.));
#9708=CARTESIAN_POINT('',(25.,-20.,26.));
#9709=CARTESIAN_POINT('',(-20.,-19.,27.));
#9710=CARTESIAN_POINT('Origin',(25.,-19.5,30.));
#9711=CARTESIAN_POINT('',(28.,-19.,30.));
#9712=CARTESIAN_POINT('',(29.,-20.,30.));
#9713=CARTESIAN_POINT('Origin',(25.,-19.,30.));
#9714=CARTESIAN_POINT('Origin',(28.5,-19.5,21.));
#9715=CARTESIAN_POINT('',(28.,-19.,80.));
#9716=CARTESIAN_POINT('',(29.,-20.,80.));
#9717=CARTESIAN_POINT('',(28.,-19.,21.));
#9718=CARTESIAN_POINT('Origin',(25.,-19.5,80.));
#9719=CARTESIAN_POINT('',(25.,-19.,83.));
#9720=CARTESIAN_POINT('',(25.,-20.,84.));
#9721=CARTESIAN_POINT('Origin',(25.,-19.,80.));
#9722=CARTESIAN_POINT('Origin',(-20.,-19.5,83.5));
#9723=CARTESIAN_POINT('',(-20.,-19.,83.));
#9724=CARTESIAN_POINT('Origin',(28.,-21.,27.));
#9725=CARTESIAN_POINT('',(28.,28.,80.));
#9726=CARTESIAN_POINT('',(28.,-8.75,80.));
#9727=CARTESIAN_POINT('',(28.,28.,30.));
#9728=CARTESIAN_POINT('',(28.,28.,27.));
#9729=CARTESIAN_POINT('',(28.,-8.75,30.));
#9730=CARTESIAN_POINT('Origin',(25.,-8.75,80.));
#9731=CARTESIAN_POINT('',(25.,28.,83.));
#9732=CARTESIAN_POINT('',(25.,-8.75,83.));
#9733=CARTESIAN_POINT('Origin',(25.,28.,80.));
#9734=CARTESIAN_POINT('Origin',(0.,3.5,83.));
#9735=CARTESIAN_POINT('',(-25.,28.,83.));
#9736=CARTESIAN_POINT('',(-25.,15.75,83.));
#9737=CARTESIAN_POINT('',(28.,28.,83.));
#9738=CARTESIAN_POINT('Origin',(-25.,15.75,80.));
#9739=CARTESIAN_POINT('',(-28.,28.,80.));
#9740=CARTESIAN_POINT('',(-28.,15.75,80.));
#9741=CARTESIAN_POINT('Origin',(-25.,28.,80.));
#9742=CARTESIAN_POINT('Origin',(28.,28.,27.));
#9743=CARTESIAN_POINT('',(-28.,28.,30.));
#9744=CARTESIAN_POINT('',(-28.,28.,27.));
#9745=CARTESIAN_POINT('',(-25.,28.,27.));
#9746=CARTESIAN_POINT('Origin',(-25.,28.,30.));
#9747=CARTESIAN_POINT('',(25.,28.,27.));
#9748=CARTESIAN_POINT('',(28.,28.,27.));
#9749=CARTESIAN_POINT('Origin',(25.,28.,30.));
#9750=CARTESIAN_POINT('Origin',(-28.,28.,27.));
#9751=CARTESIAN_POINT('',(-28.,15.75,30.));
#9752=CARTESIAN_POINT('Origin',(-25.,15.75,30.));
#9753=CARTESIAN_POINT('',(-25.,15.75,27.));
#9754=CARTESIAN_POINT('Origin',(25.,-8.75,30.));
#9755=CARTESIAN_POINT('',(25.,-8.75,27.));
#9756=CARTESIAN_POINT('Origin',(0.,3.5,27.));
#9757=CARTESIAN_POINT('Origin',(38.,-5.,93.));
#9758=CARTESIAN_POINT('',(38.,-5.,95.));
#9759=CARTESIAN_POINT('',(40.,-5.,93.));
#9760=CARTESIAN_POINT('Origin',(40.,-20.,15.));
#9761=CARTESIAN_POINT('',(40.,-5.,17.));
#9762=CARTESIAN_POINT('Origin',(38.,-5.,17.));
#9763=CARTESIAN_POINT('Origin',(0.,10.,95.));
#9764=CARTESIAN_POINT('',(0.,0.,0.));
#9765=CARTESIAN_POINT('Origin',(13.3251262658471,0.,0.));
#9766=CARTESIAN_POINT('',(14.7056733117529,-13.405863146671,4.41802289075134E-12));
#9767=CARTESIAN_POINT('',(10.5501326772895,-9.61762388247333,-2.19193273745671E-10));
#9768=CARTESIAN_POINT('',(13.3251262658471,-12.1473403730037,-1.48762015059523E-15));
#9769=CARTESIAN_POINT('',(10.0502525316942,-9.05620683581208,1.38781479615277));
#9770=CARTESIAN_POINT('Ctrl Pts',(14.7056733117529,-13.405863146671,8.83775691518096E-12));
#9771=CARTESIAN_POINT('Ctrl Pts',(14.1100932095804,-12.8629253856219,0.176689529340777));
#9772=CARTESIAN_POINT('Ctrl Pts',(13.5158390354049,-12.3177128141581,0.353880322328605));
#9773=CARTESIAN_POINT('Ctrl Pts',(11.9766359241915,-10.8925118431821,0.813848738908495));
#9774=CARTESIAN_POINT('Ctrl Pts',(10.9888514793465,-9.96433939118444,1.11043953280469));
#9775=CARTESIAN_POINT('Ctrl Pts',(10.0502525316942,-9.05620683581207,1.38781479615277));
#9776=CARTESIAN_POINT('',(10.0502525316942,-9.15961421508102,0.205863042617261));
#9777=CARTESIAN_POINT('Origin',(10.0502525316942,0.,0.));
#9778=CARTESIAN_POINT('Ctrl Pts',(10.0502525316942,-9.15961421508102,0.20586304261726));
#9779=CARTESIAN_POINT('Ctrl Pts',(10.215181575916,-9.311523886516,0.138211917211072));
#9780=CARTESIAN_POINT('Ctrl Pts',(10.3819612210757,-9.46431682339903,0.0694917893468868));
#9781=CARTESIAN_POINT('Ctrl Pts',(10.5501326772895,-9.61762388247333,-4.38387486034753E-10));
#9782=CARTESIAN_POINT('Origin',(24.5,-9.875,0.));
#9783=CARTESIAN_POINT('',(22.2,-10.,0.));
#9784=CARTESIAN_POINT('',(24.5,-9.78106229945361,2.08106229945361));
#9785=CARTESIAN_POINT('Ctrl Pts',(22.2,-10.,-3.46944695195361E-17));
#9786=CARTESIAN_POINT('Ctrl Pts',(22.2,-10.,0.279281663145492));
#9787=CARTESIAN_POINT('Ctrl Pts',(22.2664319537276,-9.98711221417022,0.57235161892421));
#9788=CARTESIAN_POINT('Ctrl Pts',(22.5234308581959,-9.94287664809831,1.09963640431428));
#9789=CARTESIAN_POINT('Ctrl Pts',(22.7136761128309,-9.91228969341567,1.33407151029786));
#9790=CARTESIAN_POINT('Ctrl Pts',(23.1318392128932,-9.8577299734025,1.69022028358443));
#9791=CARTESIAN_POINT('Ctrl Pts',(23.3865793433932,-9.82998540360157,1.83883276387722));
#9792=CARTESIAN_POINT('Ctrl Pts',(23.9342975404997,-9.79141246827269,2.03424683169264));
#9793=CARTESIAN_POINT('Ctrl Pts',(24.2273042269987,-9.78106229945361,2.08106229945361));
#9794=CARTESIAN_POINT('Ctrl Pts',(24.5,-9.78106229945361,2.08106229945361));
#9795=CARTESIAN_POINT('',(26.8,-10.,0.));
#9796=CARTESIAN_POINT('Ctrl Pts',(26.8,-10.,1.04083408558608E-15));
#9797=CARTESIAN_POINT('Ctrl Pts',(26.8,-10.,-0.279281663145491));
#9798=CARTESIAN_POINT('Ctrl Pts',(26.7335680462724,-9.98711221417022,-0.57235161892421));
#9799=CARTESIAN_POINT('Ctrl Pts',(26.4765691418041,-9.94287664809831,-1.09963640431428));
#9800=CARTESIAN_POINT('Ctrl Pts',(26.2863238871692,-9.91228969341567,-1.33407151029786));
#9801=CARTESIAN_POINT('Ctrl Pts',(25.8681607871068,-9.8577299734025,-1.69022028358443));
#9802=CARTESIAN_POINT('Ctrl Pts',(25.6134206566068,-9.82998540360157,-1.83883276387722));
#9803=CARTESIAN_POINT('Ctrl Pts',(25.0657024595003,-9.79141246827269,-2.03424683169264));
#9804=CARTESIAN_POINT('Ctrl Pts',(24.7726957730013,-9.78106229945362,-2.08106229945361));
#9805=CARTESIAN_POINT('Ctrl Pts',(24.5,-9.78106229945362,-2.08106229945361));
#9806=CARTESIAN_POINT('Ctrl Pts',(24.2273042269987,-9.78106229945362,-2.08106229945361));
#9807=CARTESIAN_POINT('Ctrl Pts',(23.9342975404997,-9.79141246827269,-2.03424683169264));
#9808=CARTESIAN_POINT('Ctrl Pts',(23.3865793433932,-9.82998540360157,-1.83883276387722));
#9809=CARTESIAN_POINT('Ctrl Pts',(23.1318392128932,-9.8577299734025,-1.69022028358443));
#9810=CARTESIAN_POINT('Ctrl Pts',(22.7136761128309,-9.91228969341567,-1.33407151029786));
#9811=CARTESIAN_POINT('Ctrl Pts',(22.5234308581959,-9.94287664809831,-1.09963640431428));
#9812=CARTESIAN_POINT('Ctrl Pts',(22.2664319537276,-9.98711221417022,-0.572351618924211));
#9813=CARTESIAN_POINT('Ctrl Pts',(22.2,-10.,-0.279281663145492));
#9814=CARTESIAN_POINT('Ctrl Pts',(22.2,-10.,4.85722573273506E-16));
#9815=CARTESIAN_POINT('Ctrl Pts',(24.5,-9.78106229945361,2.08106229945361));
#9816=CARTESIAN_POINT('Ctrl Pts',(24.7726957730013,-9.78106229945361,2.08106229945361));
#9817=CARTESIAN_POINT('Ctrl Pts',(25.0657024595003,-9.79141246827269,2.03424683169264));
#9818=CARTESIAN_POINT('Ctrl Pts',(25.6134206566068,-9.82998540360157,1.83883276387722));
#9819=CARTESIAN_POINT('Ctrl Pts',(25.8681607871068,-9.8577299734025,1.69022028358443));
#9820=CARTESIAN_POINT('Ctrl Pts',(26.2863238871692,-9.91228969341567,1.33407151029786));
#9821=CARTESIAN_POINT('Ctrl Pts',(26.4765691418041,-9.94287664809831,1.09963640431428));
#9822=CARTESIAN_POINT('Ctrl Pts',(26.7335680462724,-9.98711221417022,0.572351618924211));
#9823=CARTESIAN_POINT('Ctrl Pts',(26.8,-10.,0.279281663145492));
#9824=CARTESIAN_POINT('Ctrl Pts',(26.8,-10.,-2.08166817117217E-16));
#9825=CARTESIAN_POINT('',(24.5,-9.75,2.05));
#9826=CARTESIAN_POINT('',(24.5,-9.875,2.175));
#9827=CARTESIAN_POINT('Origin',(24.5,-9.75,0.));
#9828=CARTESIAN_POINT('Origin',(24.5,-7.75,0.));
#9829=CARTESIAN_POINT('',(24.5,-5.66552071746278,2.05));
#9830=CARTESIAN_POINT('',(24.5,-7.75,2.05));
#9831=CARTESIAN_POINT('',(26.55,-6.025,-3.34230378723604E-16));
#9832=CARTESIAN_POINT('Ctrl Pts',(26.55,-6.025,1.38777878078145E-16));
#9833=CARTESIAN_POINT('Ctrl Pts',(26.55,-6.025,0.259594733817565));
#9834=CARTESIAN_POINT('Ctrl Pts',(26.4976983668916,-6.00658123724956,0.535111320788412));
#9835=CARTESIAN_POINT('Ctrl Pts',(26.287830413716,-5.94008056213222,1.03961781502895));
#9836=CARTESIAN_POINT('Ctrl Pts',(26.13037388806,-5.8928399020443,1.26876391480488));
#9837=CARTESIAN_POINT('Ctrl Pts',(25.7686724003374,-5.80318375449856,1.63046540252745));
#9838=CARTESIAN_POINT('Ctrl Pts',(25.5395625840329,-5.75468697285078,1.78785157007388));
#9839=CARTESIAN_POINT('Ctrl Pts',(25.035191264494,-5.68525838031662,1.99766693028397));
#9840=CARTESIAN_POINT('Ctrl Pts',(24.7597261277258,-5.66552071746278,2.05));
#9841=CARTESIAN_POINT('Ctrl Pts',(24.5,-5.66552071746278,2.05));
#9842=CARTESIAN_POINT('',(22.45,-6.025,-6.81175073918965E-16));
#9843=CARTESIAN_POINT('Ctrl Pts',(22.45,-6.025,-6.24500451351651E-16));
#9844=CARTESIAN_POINT('Ctrl Pts',(22.45,-6.025,-0.259594733817566));
#9845=CARTESIAN_POINT('Ctrl Pts',(22.5023016331084,-6.00658123724956,-0.535111320788414));
#9846=CARTESIAN_POINT('Ctrl Pts',(22.712169586284,-5.94008056213222,-1.03961781502895));
#9847=CARTESIAN_POINT('Ctrl Pts',(22.86962611194,-5.8928399020443,-1.26876391480488));
#9848=CARTESIAN_POINT('Ctrl Pts',(23.2313275996626,-5.80318375449856,-1.63046540252745));
#9849=CARTESIAN_POINT('Ctrl Pts',(23.4604374159671,-5.75468697285078,-1.78785157007388));
#9850=CARTESIAN_POINT('Ctrl Pts',(23.964808735506,-5.68525838031662,-1.99766693028397));
#9851=CARTESIAN_POINT('Ctrl Pts',(24.2402738722742,-5.66552071746278,-2.05));
#9852=CARTESIAN_POINT('Ctrl Pts',(24.7597261277258,-5.66552071746278,-2.05));
#9853=CARTESIAN_POINT('Ctrl Pts',(25.035191264494,-5.68525838031662,-1.99766693028397));
#9854=CARTESIAN_POINT('Ctrl Pts',(25.5395625840329,-5.75468697285078,-1.78785157007388));
#9855=CARTESIAN_POINT('Ctrl Pts',(25.7686724003374,-5.80318375449856,-1.63046540252745));
#9856=CARTESIAN_POINT('Ctrl Pts',(26.13037388806,-5.8928399020443,-1.26876391480488));
#9857=CARTESIAN_POINT('Ctrl Pts',(26.287830413716,-5.94008056213222,-1.03961781502895));
#9858=CARTESIAN_POINT('Ctrl Pts',(26.4976983668916,-6.00658123724956,-0.535111320788414));
#9859=CARTESIAN_POINT('Ctrl Pts',(26.55,-6.025,-0.259594733817566));
#9860=CARTESIAN_POINT('Ctrl Pts',(26.55,-6.025,-6.24500451351651E-16));
#9861=CARTESIAN_POINT('Ctrl Pts',(24.5,-5.66552071746278,2.05));
#9862=CARTESIAN_POINT('Ctrl Pts',(24.2402738722742,-5.66552071746278,2.05));
#9863=CARTESIAN_POINT('Ctrl Pts',(23.964808735506,-5.68525838031662,1.99766693028397));
#9864=CARTESIAN_POINT('Ctrl Pts',(23.4604374159671,-5.75468697285078,1.78785157007388));
#9865=CARTESIAN_POINT('Ctrl Pts',(23.2313275996626,-5.80318375449856,1.63046540252745));
#9866=CARTESIAN_POINT('Ctrl Pts',(22.86962611194,-5.8928399020443,1.26876391480488));
#9867=CARTESIAN_POINT('Ctrl Pts',(22.712169586284,-5.94008056213222,1.03961781502895));
#9868=CARTESIAN_POINT('Ctrl Pts',(22.5023016331084,-6.00658123724956,0.535111320788414));
#9869=CARTESIAN_POINT('Ctrl Pts',(22.45,-6.025,0.259594733817566));
#9870=CARTESIAN_POINT('Ctrl Pts',(22.45,-6.025,0.));
#9871=CARTESIAN_POINT('Origin',(24.5,0.,9.875));
#9872=CARTESIAN_POINT('',(22.2,0.,10.));
#9873=CARTESIAN_POINT('',(26.8,0.,10.));
#9874=CARTESIAN_POINT('Ctrl Pts',(22.2,-2.77555756156289E-16,10.));
#9875=CARTESIAN_POINT('Ctrl Pts',(22.2,0.279281663145492,10.));
#9876=CARTESIAN_POINT('Ctrl Pts',(22.2664319537276,0.57235161892421,9.98711221417022));
#9877=CARTESIAN_POINT('Ctrl Pts',(22.5234308581959,1.09963640431428,9.94287664809831));
#9878=CARTESIAN_POINT('Ctrl Pts',(22.7136761128309,1.33407151029786,9.91228969341567));
#9879=CARTESIAN_POINT('Ctrl Pts',(23.1318392128932,1.69022028358443,9.8577299734025));
#9880=CARTESIAN_POINT('Ctrl Pts',(23.3865793433932,1.83883276387722,9.82998540360157));
#9881=CARTESIAN_POINT('Ctrl Pts',(23.9342975404997,2.03424683169264,9.79141246827269));
#9882=CARTESIAN_POINT('Ctrl Pts',(24.2273042269987,2.08106229945361,9.78106229945362));
#9883=CARTESIAN_POINT('Ctrl Pts',(24.7726957730013,2.08106229945361,9.78106229945362));
#9884=CARTESIAN_POINT('Ctrl Pts',(25.0657024595003,2.03424683169264,9.79141246827269));
#9885=CARTESIAN_POINT('Ctrl Pts',(25.6134206566068,1.83883276387722,9.82998540360157));
#9886=CARTESIAN_POINT('Ctrl Pts',(25.8681607871068,1.69022028358443,9.8577299734025));
#9887=CARTESIAN_POINT('Ctrl Pts',(26.2863238871692,1.33407151029786,9.91228969341567));
#9888=CARTESIAN_POINT('Ctrl Pts',(26.4765691418041,1.09963640431428,9.94287664809831));
#9889=CARTESIAN_POINT('Ctrl Pts',(26.7335680462724,0.572351618924211,9.98711221417022));
#9890=CARTESIAN_POINT('Ctrl Pts',(26.8,0.279281663145492,10.));
#9891=CARTESIAN_POINT('Ctrl Pts',(26.8,0.,10.));
#9892=CARTESIAN_POINT('',(22.45,2.51052593825207E-16,9.75));
#9893=CARTESIAN_POINT('',(22.325,2.66360678814549E-16,9.875));
#9894=CARTESIAN_POINT('Origin',(24.5,0.,9.75));
#9895=CARTESIAN_POINT('Ctrl Pts',(26.8,1.31838984174237E-15,10.));
#9896=CARTESIAN_POINT('Ctrl Pts',(26.8,-0.279281663145491,10.));
#9897=CARTESIAN_POINT('Ctrl Pts',(26.7335680462724,-0.572351618924209,9.98711221417022));
#9898=CARTESIAN_POINT('Ctrl Pts',(26.4765691418041,-1.09963640431428,9.94287664809831));
#9899=CARTESIAN_POINT('Ctrl Pts',(26.2863238871692,-1.33407151029786,9.91228969341567));
#9900=CARTESIAN_POINT('Ctrl Pts',(25.8681607871068,-1.69022028358443,9.8577299734025));
#9901=CARTESIAN_POINT('Ctrl Pts',(25.6134206566068,-1.83883276387722,9.82998540360157));
#9902=CARTESIAN_POINT('Ctrl Pts',(25.0657024595003,-2.03424683169264,9.79141246827269));
#9903=CARTESIAN_POINT('Ctrl Pts',(24.7726957730013,-2.08106229945361,9.78106229945362));
#9904=CARTESIAN_POINT('Ctrl Pts',(24.5,-2.08106229945361,9.78106229945362));
#9905=CARTESIAN_POINT('Ctrl Pts',(24.2273042269987,-2.08106229945361,9.78106229945362));
#9906=CARTESIAN_POINT('Ctrl Pts',(23.9342975404997,-2.03424683169264,9.79141246827269));
#9907=CARTESIAN_POINT('Ctrl Pts',(23.3865793433932,-1.83883276387722,9.82998540360157));
#9908=CARTESIAN_POINT('Ctrl Pts',(23.1318392128932,-1.69022028358443,9.8577299734025));
#9909=CARTESIAN_POINT('Ctrl Pts',(22.7136761128309,-1.33407151029786,9.91228969341567));
#9910=CARTESIAN_POINT('Ctrl Pts',(22.5234308581959,-1.09963640431428,9.94287664809831));
#9911=CARTESIAN_POINT('Ctrl Pts',(22.2664319537276,-0.572351618924211,9.98711221417022));
#9912=CARTESIAN_POINT('Ctrl Pts',(22.2,-0.279281663145492,10.));
#9913=CARTESIAN_POINT('Ctrl Pts',(22.2,3.46944695195361E-16,10.));
#9914=CARTESIAN_POINT('Origin',(24.5,0.,7.75));
#9915=CARTESIAN_POINT('',(22.45,1.94915235951676E-16,6.025));
#9916=CARTESIAN_POINT('',(22.45,2.51052593825207E-16,7.75));
#9917=CARTESIAN_POINT('',(24.5,2.05,5.66552071746278));
#9918=CARTESIAN_POINT('Ctrl Pts',(24.5,2.05,5.66552071746278));
#9919=CARTESIAN_POINT('Ctrl Pts',(24.2402738722742,2.05,5.66552071746278));
#9920=CARTESIAN_POINT('Ctrl Pts',(23.964808735506,1.99766693028397,5.68525838031662));
#9921=CARTESIAN_POINT('Ctrl Pts',(23.4604374159671,1.78785157007388,5.75468697285078));
#9922=CARTESIAN_POINT('Ctrl Pts',(23.2313275996626,1.63046540252745,5.80318375449856));
#9923=CARTESIAN_POINT('Ctrl Pts',(22.86962611194,1.26876391480488,5.8928399020443));
#9924=CARTESIAN_POINT('Ctrl Pts',(22.712169586284,1.03961781502895,5.94008056213222));
#9925=CARTESIAN_POINT('Ctrl Pts',(22.5023016331084,0.535111320788414,6.00658123724956));
#9926=CARTESIAN_POINT('Ctrl Pts',(22.45,0.259594733817566,6.025));
#9927=CARTESIAN_POINT('Ctrl Pts',(22.45,2.77555756156289E-16,6.025));
#9928=CARTESIAN_POINT('Ctrl Pts',(22.45,2.08166817117217E-16,6.025));
#9929=CARTESIAN_POINT('Ctrl Pts',(22.45,-0.259594733817565,6.025));
#9930=CARTESIAN_POINT('Ctrl Pts',(22.5023016331084,-0.535111320788413,6.00658123724956));
#9931=CARTESIAN_POINT('Ctrl Pts',(22.712169586284,-1.03961781502895,5.94008056213222));
#9932=CARTESIAN_POINT('Ctrl Pts',(22.86962611194,-1.26876391480488,5.8928399020443));
#9933=CARTESIAN_POINT('Ctrl Pts',(23.2313275996626,-1.63046540252745,5.80318375449856));
#9934=CARTESIAN_POINT('Ctrl Pts',(23.4604374159671,-1.78785157007388,5.75468697285078));
#9935=CARTESIAN_POINT('Ctrl Pts',(23.964808735506,-1.99766693028397,5.68525838031662));
#9936=CARTESIAN_POINT('Ctrl Pts',(24.2402738722742,-2.05,5.66552071746278));
#9937=CARTESIAN_POINT('Ctrl Pts',(24.7597261277258,-2.05,5.66552071746278));
#9938=CARTESIAN_POINT('Ctrl Pts',(25.035191264494,-1.99766693028397,5.68525838031662));
#9939=CARTESIAN_POINT('Ctrl Pts',(25.5395625840329,-1.78785157007388,5.75468697285078));
#9940=CARTESIAN_POINT('Ctrl Pts',(25.7686724003374,-1.63046540252745,5.80318375449856));
#9941=CARTESIAN_POINT('Ctrl Pts',(26.13037388806,-1.26876391480488,5.8928399020443));
#9942=CARTESIAN_POINT('Ctrl Pts',(26.287830413716,-1.03961781502895,5.94008056213222));
#9943=CARTESIAN_POINT('Ctrl Pts',(26.4976983668916,-0.535111320788413,6.00658123724956));
#9944=CARTESIAN_POINT('Ctrl Pts',(26.55,-0.259594733817566,6.025));
#9945=CARTESIAN_POINT('Ctrl Pts',(26.55,0.259594733817565,6.025));
#9946=CARTESIAN_POINT('Ctrl Pts',(26.4976983668916,0.535111320788412,6.00658123724956));
#9947=CARTESIAN_POINT('Ctrl Pts',(26.287830413716,1.03961781502895,5.94008056213222));
#9948=CARTESIAN_POINT('Ctrl Pts',(26.13037388806,1.26876391480488,5.8928399020443));
#9949=CARTESIAN_POINT('Ctrl Pts',(25.7686724003374,1.63046540252745,5.80318375449856));
#9950=CARTESIAN_POINT('Ctrl Pts',(25.5395625840329,1.78785157007388,5.75468697285078));
#9951=CARTESIAN_POINT('Ctrl Pts',(25.035191264494,1.99766693028397,5.68525838031662));
#9952=CARTESIAN_POINT('Ctrl Pts',(24.7597261277258,2.05,5.66552071746278));
#9953=CARTESIAN_POINT('Ctrl Pts',(24.5,2.05,5.66552071746278));
#9954=CARTESIAN_POINT('Origin',(10.3002525316942,0.,0.));
#9955=CARTESIAN_POINT('',(10.0502525316942,6.525,-7.99082036443648E-16));
#9956=CARTESIAN_POINT('Origin',(10.0502525316942,0.,0.));
#9957=CARTESIAN_POINT('',(10.5502525316942,6.025,7.3784969648628E-16));
#9958=CARTESIAN_POINT('',(10.3002525316942,6.275,-7.68465866464964E-16));
#9959=CARTESIAN_POINT('',(10.5502525316942,-6.025,-7.3784969648628E-16));
#9960=CARTESIAN_POINT('Origin',(10.5502525316942,0.,0.));
#9961=CARTESIAN_POINT('Origin',(10.5502525316942,0.,0.));
#9962=CARTESIAN_POINT('Origin',(19.7001262658471,0.,0.));
#9963=CARTESIAN_POINT('',(28.85,6.025,-7.3784969648628E-16));
#9964=CARTESIAN_POINT('',(28.85,-6.025,-7.3784969648628E-16));
#9965=CARTESIAN_POINT('Origin',(28.85,0.,0.));
#9966=CARTESIAN_POINT('Origin',(28.85,0.,0.));
#9967=CARTESIAN_POINT('',(19.7001262658471,-6.025,-7.3784969648628E-16));
#9968=CARTESIAN_POINT('',(19.7001262658471,-6.025,-7.3784969648628E-16));
#9969=CARTESIAN_POINT('Origin',(10.0502525316942,9.16192731696939,0.));
#9970=CARTESIAN_POINT('',(10.0502525316942,8.18410616705958,-4.11841212213243));
#9971=CARTESIAN_POINT('',(10.0502525316942,8.64769560732005,-3.02626384252387));
#9972=CARTESIAN_POINT('Origin',(10.0502525316942,0.,0.));
#9973=CARTESIAN_POINT('',(10.0502525316942,9.2755658561365,-5.45537535466284));
#9974=CARTESIAN_POINT('Ctrl Pts',(10.0502525316942,8.18410616705958,-4.11841212213243));
#9975=CARTESIAN_POINT('Ctrl Pts',(10.0502525316942,8.19431842617809,-4.12237383820348));
#9976=CARTESIAN_POINT('Ctrl Pts',(10.0502525316942,8.21464735012275,-4.1304870856583));
#9977=CARTESIAN_POINT('Ctrl Pts',(10.0502525316942,8.24485395393399,-4.14322640185693));
#9978=CARTESIAN_POINT('Ctrl Pts',(10.0502525316942,8.28455481633258,-4.16135311687778));
#9979=CARTESIAN_POINT('Ctrl Pts',(10.0502525316942,8.33321297157003,-4.18592891379899));
#9980=CARTESIAN_POINT('Ctrl Pts',(10.0502525316942,8.38088287416164,-4.21244876582417));
#9981=CARTESIAN_POINT('Ctrl Pts',(10.0502525316942,8.42753204825146,-4.24094982636281));
#9982=CARTESIAN_POINT('Ctrl Pts',(10.0502525316942,8.47311320506822,-4.27147990109806));
#9983=CARTESIAN_POINT('Ctrl Pts',(10.0502525316942,8.51756357237276,-4.3040953182409));
#9984=CARTESIAN_POINT('Ctrl Pts',(10.0502525316942,8.56081999110915,-4.33884232599626));
#9985=CARTESIAN_POINT('Ctrl Pts',(10.0502525316942,8.60283329387128,-4.37573883085758));
#9986=CARTESIAN_POINT('Ctrl Pts',(10.0502525316942,8.6435823082099,-4.41475679767577));
#9987=CARTESIAN_POINT('Ctrl Pts',(10.0502525316942,8.68309075792173,-4.45580026211617));
#9988=CARTESIAN_POINT('Ctrl Pts',(10.0502525316942,8.72143659100306,-4.4986943294444));
#9989=CARTESIAN_POINT('Ctrl Pts',(10.0502525316942,8.75872782924178,-4.54322265243728));
#9990=CARTESIAN_POINT('Ctrl Pts',(10.0502525316942,8.79508318101477,-4.58915808705618));
#9991=CARTESIAN_POINT('Ctrl Pts',(10.0502525316942,8.83061212429863,-4.63629390238203));
#9992=CARTESIAN_POINT('Ctrl Pts',(10.0502525316942,8.86539310688376,-4.68447828052063));
#9993=CARTESIAN_POINT('Ctrl Pts',(10.0502525316942,8.89945965089929,-4.73363584056076));
#9994=CARTESIAN_POINT('Ctrl Pts',(10.0502525316942,8.93281562325407,-4.78374147310216));
#9995=CARTESIAN_POINT('Ctrl Pts',(10.0502525316942,8.96544592744964,-4.83480166455838));
#9996=CARTESIAN_POINT('Ctrl Pts',(10.0502525316942,8.99732855257362,-4.88683372770265));
#9997=CARTESIAN_POINT('Ctrl Pts',(10.0502525316942,9.02844713284016,-4.9398440174493));
#9998=CARTESIAN_POINT('Ctrl Pts',(10.0502525316942,9.05880038387882,-4.99381190670161));
#9999=CARTESIAN_POINT('Ctrl Pts',(10.0502525316942,9.08839676934597,-5.04870046735128));
#10000=CARTESIAN_POINT('Ctrl Pts',(10.0502525316942,9.11725155657582,-5.10446294828982));
#10001=CARTESIAN_POINT('Ctrl Pts',(10.0502525316942,9.14538320175401,-5.16105047473192));
#10002=CARTESIAN_POINT('Ctrl Pts',(10.0502525316942,9.17281011362288,-5.21841931731543));
#10003=CARTESIAN_POINT('Ctrl Pts',(10.0502525316942,9.19954772791879,-5.27653724822262));
#10004=CARTESIAN_POINT('Ctrl Pts',(10.0502525316942,9.2256083913841,-5.33538160688598));
#10005=CARTESIAN_POINT('Ctrl Pts',(10.0502525316942,9.24592251158686,-5.38302685274804));
#10006=CARTESIAN_POINT('Ctrl Pts',(10.0502525316942,9.26085993003723,-5.41907797515233));
#10007=CARTESIAN_POINT('Ctrl Pts',(10.0502525316942,9.27068592765741,-5.44325277512453));
#10008=CARTESIAN_POINT('Ctrl Pts',(10.0502525316942,9.2755658561365,-5.45537535466284));
#10009=CARTESIAN_POINT('',(10.0502525316942,7.28928030147641,-5.55043285230422));
#10010=CARTESIAN_POINT('Ctrl Pts',(10.0502525316942,9.2755658561365,-5.45537535466284));
#10011=CARTESIAN_POINT('Ctrl Pts',(10.0502525316942,9.25004353985722,-5.48408843121132));
#10012=CARTESIAN_POINT('Ctrl Pts',(10.0502525316942,9.19987743117415,-5.53944326709657));
#10013=CARTESIAN_POINT('Ctrl Pts',(10.0502525316942,9.12726384869626,-5.61626154813455));
#10014=CARTESIAN_POINT('Ctrl Pts',(10.0502525316942,9.03572636773682,-5.70623565557996));
#10015=CARTESIAN_POINT('Ctrl Pts',(10.0502525316942,8.93010252395574,-5.79796105654696));
#10016=CARTESIAN_POINT('Ctrl Pts',(10.0502525316942,8.83316895299322,-5.86920138549131));
#10017=CARTESIAN_POINT('Ctrl Pts',(10.0502525316942,8.74463793548674,-5.92064129305387));
#10018=CARTESIAN_POINT('Ctrl Pts',(10.0502525316942,8.6639539190358,-5.95360120899604));
#10019=CARTESIAN_POINT('Ctrl Pts',(10.0502525316942,8.59022668922188,-5.97019580138365));
#10020=CARTESIAN_POINT('Ctrl Pts',(10.0502525316942,8.52210226517413,-5.97364002234323));
#10021=CARTESIAN_POINT('Ctrl Pts',(10.0502525316942,8.45790665865659,-5.96790845784416));
#10022=CARTESIAN_POINT('Ctrl Pts',(10.0502525316942,8.39592031140414,-5.95708504467347));
#10023=CARTESIAN_POINT('Ctrl Pts',(10.0502525316942,8.33461788057945,-5.94479472837688));
#10024=CARTESIAN_POINT('Ctrl Pts',(10.0502525316942,8.27290485770376,-5.93364300051867));
#10025=CARTESIAN_POINT('Ctrl Pts',(10.0502525316942,8.2104048870761,-5.92453426026728));
#10026=CARTESIAN_POINT('Ctrl Pts',(10.0502525316942,8.14730848207823,-5.91703766966772));
#10027=CARTESIAN_POINT('Ctrl Pts',(10.0502525316942,8.08413710664289,-5.90995523970614));
#10028=CARTESIAN_POINT('Ctrl Pts',(10.0502525316942,8.02154163982398,-5.90180775582857));
#10029=CARTESIAN_POINT('Ctrl Pts',(10.0502525316942,7.96008352176745,-5.89136254542228));
#10030=CARTESIAN_POINT('Ctrl Pts',(10.0502525316942,7.90003527315714,-5.87811409765682));
#10031=CARTESIAN_POINT('Ctrl Pts',(10.0502525316942,7.84146798659238,-5.86206014174823));
#10032=CARTESIAN_POINT('Ctrl Pts',(10.0502525316942,7.78432826524869,-5.84350339850201));
#10033=CARTESIAN_POINT('Ctrl Pts',(10.0502525316942,7.72851334381364,-5.82285820956226));
#10034=CARTESIAN_POINT('Ctrl Pts',(10.0502525316942,7.67395636265026,-5.80043066085533));
#10035=CARTESIAN_POINT('Ctrl Pts',(10.0502525316942,7.62067331151744,-5.77629688888814));
#10036=CARTESIAN_POINT('Ctrl Pts',(10.0502525316942,7.56872566186653,-5.75039773581461));
#10037=CARTESIAN_POINT('Ctrl Pts',(10.0502525316942,7.51819950516883,-5.72259034420254));
#10038=CARTESIAN_POINT('Ctrl Pts',(10.0502525316942,7.46918012077942,-5.69271190798352));
#10039=CARTESIAN_POINT('Ctrl Pts',(10.0502525316942,7.42172307293681,-5.66064997807339));
#10040=CARTESIAN_POINT('Ctrl Pts',(10.0502525316942,7.37585243997691,-5.62635178473812));
#10041=CARTESIAN_POINT('Ctrl Pts',(10.0502525316942,7.34042983445952,-5.59710957827922));
#10042=CARTESIAN_POINT('Ctrl Pts',(10.0502525316942,7.31457760934185,-5.5741645986968));
#10043=CARTESIAN_POINT('Ctrl Pts',(10.0502525316942,7.2976598885924,-5.55841836363355));
#10044=CARTESIAN_POINT('Ctrl Pts',(10.0502525316942,7.28928030147641,-5.55043285230422));
#10045=CARTESIAN_POINT('',(10.0502525316942,6.51088816465465,-6.44587057493322));
#10046=CARTESIAN_POINT('Origin',(10.0502525316942,0.,0.));
#10047=CARTESIAN_POINT('',(10.0502525316942,7.13578365451837,-8.05467776187827));
#10048=CARTESIAN_POINT('Ctrl Pts',(10.0502525316942,6.51088816465465,-6.44587057493322));
#10049=CARTESIAN_POINT('Ctrl Pts',(10.0502525316942,6.51937636264256,-6.45279415243689));
#10050=CARTESIAN_POINT('Ctrl Pts',(10.0502525316942,6.5362031868863,-6.46679229227336));
#10051=CARTESIAN_POINT('Ctrl Pts',(10.0502525316942,6.56099470907402,-6.48824245587723));
#10052=CARTESIAN_POINT('Ctrl Pts',(10.0502525316942,6.59315100996711,-6.51775022748935));
#10053=CARTESIAN_POINT('Ctrl Pts',(10.0502525316942,6.63183332667763,-6.55615939617772));
#10054=CARTESIAN_POINT('Ctrl Pts',(10.0502525316942,6.66897501320444,-6.59611208427845));
#10055=CARTESIAN_POINT('Ctrl Pts',(10.0502525316942,6.7045337021382,-6.63763359119236));
#10056=CARTESIAN_POINT('Ctrl Pts',(10.0502525316942,6.73844964641633,-6.68075476979194));
#10057=CARTESIAN_POINT('Ctrl Pts',(10.0502525316942,6.77064573971725,-6.72550979370064));
#10058=CARTESIAN_POINT('Ctrl Pts',(10.0502525316942,6.801047622728,-6.77192313035348));
#10059=CARTESIAN_POINT('Ctrl Pts',(10.0502525316942,6.82960300105582,-6.81999661627367));
#10060=CARTESIAN_POINT('Ctrl Pts',(10.0502525316942,6.8563004018424,-6.86969704580336));
#10061=CARTESIAN_POINT('Ctrl Pts',(10.0502525316942,6.88119204236944,-6.92094048249309));
#10062=CARTESIAN_POINT('Ctrl Pts',(10.0502525316942,6.90440610103192,-6.97358467882161));
#10063=CARTESIAN_POINT('Ctrl Pts',(10.0502525316942,6.92611216762375,-7.02745725692073));
#10064=CARTESIAN_POINT('Ctrl Pts',(10.0502525316942,6.94649333188842,-7.08237887287822));
#10065=CARTESIAN_POINT('Ctrl Pts',(10.0502525316942,6.96571759693621,-7.13818674446165));
#10066=CARTESIAN_POINT('Ctrl Pts',(10.0502525316942,6.98390648535873,-7.19476072597386));
#10067=CARTESIAN_POINT('Ctrl Pts',(10.0502525316942,7.00111517257794,-7.25203948481561));
#10068=CARTESIAN_POINT('Ctrl Pts',(10.0502525316942,7.01735509547412,-7.31000033546873));
#10069=CARTESIAN_POINT('Ctrl Pts',(10.0502525316942,7.032609892012,-7.36864478180451));
#10070=CARTESIAN_POINT('Ctrl Pts',(10.0502525316942,7.04685327862879,-7.42798248750274));
#10071=CARTESIAN_POINT('Ctrl Pts',(10.0502525316942,7.06006772676068,-7.48801443914016));
#10072=CARTESIAN_POINT('Ctrl Pts',(10.0502525316942,7.07225838902223,-7.54872062228975));
#10073=CARTESIAN_POINT('Ctrl Pts',(10.0502525316942,7.08344472624202,-7.6100685316471));
#10074=CARTESIAN_POINT('Ctrl Pts',(10.0502525316942,7.09365570540476,-7.67201842213158));
#10075=CARTESIAN_POINT('Ctrl Pts',(10.0502525316942,7.10292398252533,-7.73452951433515));
#10076=CARTESIAN_POINT('Ctrl Pts',(10.0502525316942,7.11128057847415,-7.79756590777721));
#10077=CARTESIAN_POINT('Ctrl Pts',(10.0502525316942,7.11875013245223,-7.86110172188657));
#10078=CARTESIAN_POINT('Ctrl Pts',(10.0502525316942,7.12535138940982,-7.92511922053603));
#10079=CARTESIAN_POINT('Ctrl Pts',(10.0502525316942,7.1299480751289,-7.97670995045205));
#10080=CARTESIAN_POINT('Ctrl Pts',(10.0502525316942,7.13301399479354,-8.01561252148766));
#10081=CARTESIAN_POINT('Ctrl Pts',(10.0502525316942,7.13488864983229,-8.04164052278268));
#10082=CARTESIAN_POINT('Ctrl Pts',(10.0502525316942,7.13578365451837,-8.05467776187827));
#10083=CARTESIAN_POINT('',(10.0502525316942,5.21733945232202,-7.53128682236137));
#10084=CARTESIAN_POINT('Ctrl Pts',(10.0502525316942,7.13578365451837,-8.05467776187827));
#10085=CARTESIAN_POINT('Ctrl Pts',(10.0502525316942,7.10263766069576,-8.07409869096647));
#10086=CARTESIAN_POINT('Ctrl Pts',(10.0502525316942,7.03782127112617,-8.11124208821886));
#10087=CARTESIAN_POINT('Ctrl Pts',(10.0502525316942,6.94502349601963,-8.16186178396251));
#10088=CARTESIAN_POINT('Ctrl Pts',(10.0502525316942,6.83016265001357,-8.21914560790757));
#10089=CARTESIAN_POINT('Ctrl Pts',(10.0502525316942,6.70136369739476,-8.27374208546745));
#10090=CARTESIAN_POINT('Ctrl Pts',(10.0502525316942,6.58715992075444,-8.31154154378012));
#10091=CARTESIAN_POINT('Ctrl Pts',(10.0502525316942,6.48706611403475,-8.33310621412631));
#10092=CARTESIAN_POINT('Ctrl Pts',(10.0502525316942,6.40014588026892,-8.33952022470187));
#10093=CARTESIAN_POINT('Ctrl Pts',(10.0502525316942,6.32489910686351,-8.33251965296669));
#10094=CARTESIAN_POINT('Ctrl Pts',(10.0502525316942,6.25904460664514,-8.31474369699109));
#10095=CARTESIAN_POINT('Ctrl Pts',(10.0502525316942,6.19976210758369,-8.28945512184757));
#10096=CARTESIAN_POINT('Ctrl Pts',(10.0502525316942,6.14415420671479,-8.26000660950279));
#10097=CARTESIAN_POINT('Ctrl Pts',(10.0502525316942,6.08965004701613,-8.22937433118026));
#10098=CARTESIAN_POINT('Ctrl Pts',(10.0502525316942,6.03440354789477,-8.19969803488993));
#10099=CARTESIAN_POINT('Ctrl Pts',(10.0502525316942,5.9777772990961,-8.17172155504672));
#10100=CARTESIAN_POINT('Ctrl Pts',(10.0502525316942,5.92008562586321,-8.1450940122787));
#10101=CARTESIAN_POINT('Ctrl Pts',(10.0502525316942,5.86219466883171,-8.11883719254497));
#10102=CARTESIAN_POINT('Ctrl Pts',(10.0502525316942,5.80518055320261,-8.09174541189394));
#10103=CARTESIAN_POINT('Ctrl Pts',(10.0502525316942,5.74995815707107,-8.06281982355119));
#10104=CARTESIAN_POINT('Ctrl Pts',(10.0502525316942,5.69694287444674,-8.03166387167001));
#10105=CARTESIAN_POINT('Ctrl Pts',(10.0502525316942,5.6462030201203,-7.99829736542789));
#10106=CARTESIAN_POINT('Ctrl Pts',(10.0502525316942,5.59759426482043,-7.96299170889331));
#10107=CARTESIAN_POINT('Ctrl Pts',(10.0502525316942,5.5508908343176,-7.92610920815888));
#10108=CARTESIAN_POINT('Ctrl Pts',(10.0502525316942,5.50593455556538,-7.88792030747535));
#10109=CARTESIAN_POINT('Ctrl Pts',(10.0502525316942,5.46271710825365,-7.84850235807098));
#10110=CARTESIAN_POINT('Ctrl Pts',(10.0502525316942,5.42131523598658,-7.80781809321391));
#10111=CARTESIAN_POINT('Ctrl Pts',(10.0502525316942,5.38185496199325,-7.76575825114004));
#10112=CARTESIAN_POINT('Ctrl Pts',(10.0502525316942,5.34446770160195,-7.72219434684711));
#10113=CARTESIAN_POINT('Ctrl Pts',(10.0502525316942,5.3092410482218,-7.67703660519485));
#10114=CARTESIAN_POINT('Ctrl Pts',(10.0502525316942,5.27621420845565,-7.63024227979884));
#10115=CARTESIAN_POINT('Ctrl Pts',(10.0502525316942,5.251561647403,-7.59148510170534));
#10116=CARTESIAN_POINT('Ctrl Pts',(10.0502525316942,5.23406510887067,-7.56167435245346));
#10117=CARTESIAN_POINT('Ctrl Pts',(10.0502525316942,5.22284125454301,-7.54147092977177));
#10118=CARTESIAN_POINT('Ctrl Pts',(10.0502525316942,5.21733945232202,-7.53128682236137));
#10119=CARTESIAN_POINT('',(10.0502525316942,4.20033906466803,-8.14236230483842));
#10120=CARTESIAN_POINT('Origin',(10.0502525316942,0.,0.));
#10121=CARTESIAN_POINT('',(10.0502525316942,4.29750123086779,-9.86553218952114));
#10122=CARTESIAN_POINT('Ctrl Pts',(10.0502525316942,4.20033906466803,-8.14236230483842));
#10123=CARTESIAN_POINT('Ctrl Pts',(10.0502525316942,4.20627231756552,-8.15157001576925));
#10124=CARTESIAN_POINT('Ctrl Pts',(10.0502525316942,4.21794991531197,-8.17008281252941));
#10125=CARTESIAN_POINT('Ctrl Pts',(10.0502525316942,4.23489958895176,-8.1981441320729));
#10126=CARTESIAN_POINT('Ctrl Pts',(10.0502525316942,4.2563636455618,-8.23614453399815));
#10127=CARTESIAN_POINT('Ctrl Pts',(10.0502525316942,4.28128362907021,-8.28462731741005));
#10128=CARTESIAN_POINT('Ctrl Pts',(10.0502525316942,4.30426141247364,-8.33410199410829));
#10129=CARTESIAN_POINT('Ctrl Pts',(10.0502525316942,4.32524888402656,-8.38457953300338));
#10130=CARTESIAN_POINT('Ctrl Pts',(10.0502525316942,4.34417968683382,-8.43607081406306));
#10131=CARTESIAN_POINT('Ctrl Pts',(10.0502525316942,4.36096992819547,-8.48858451117083));
#10132=CARTESIAN_POINT('Ctrl Pts',(10.0502525316942,4.37554132734911,-8.54212091594884));
#10133=CARTESIAN_POINT('Ctrl Pts',(10.0502525316942,4.38784358185488,-8.59666561517837));
#10134=CARTESIAN_POINT('Ctrl Pts',(10.0502525316942,4.39787604148868,-8.65218348309394));
#10135=CARTESIAN_POINT('Ctrl Pts',(10.0502525316942,4.4057143056259,-8.70861082741579));
#10136=CARTESIAN_POINT('Ctrl Pts',(10.0502525316942,4.41152423606579,-8.76585197201427));
#10137=CARTESIAN_POINT('Ctrl Pts',(10.0502525316942,4.41552038997766,-8.82379538192297));
#10138=CARTESIAN_POINT('Ctrl Pts',(10.0502525316942,4.41793231637186,-8.88232706878773));
#10139=CARTESIAN_POINT('Ctrl Pts',(10.0502525316942,4.41897009817737,-8.94134413332185));
#10140=CARTESIAN_POINT('Ctrl Pts',(10.0502525316942,4.41878643730905,-9.00076986272314));
#10141=CARTESIAN_POINT('Ctrl Pts',(10.0502525316942,4.41745276152696,-9.06056297636652));
#10142=CARTESIAN_POINT('Ctrl Pts',(10.0502525316942,4.41498695816126,-9.12070543323243));
#10143=CARTESIAN_POINT('Ctrl Pts',(10.0502525316942,4.4113730012699,-9.18119360744053));
#10144=CARTESIAN_POINT('Ctrl Pts',(10.0502525316942,4.40658290745794,-9.24202856762888));
#10145=CARTESIAN_POINT('Ctrl Pts',(10.0502525316942,4.40059970120156,-9.3032058354636));
#10146=CARTESIAN_POINT('Ctrl Pts',(10.0502525316942,4.3934344677265,-9.36470796833893));
#10147=CARTESIAN_POINT('Ctrl Pts',(10.0502525316942,4.38511576007206,-9.42651006560004));
#10148=CARTESIAN_POINT('Ctrl Pts',(10.0502525316942,4.37568340938316,-9.48858327871958));
#10149=CARTESIAN_POINT('Ctrl Pts',(10.0502525316942,4.36518107490567,-9.55089891543934));
#10150=CARTESIAN_POINT('Ctrl Pts',(10.0502525316942,4.35364935309914,-9.61343241834946));
#10151=CARTESIAN_POINT('Ctrl Pts',(10.0502525316942,4.34111967477257,-9.67616678749592));
#10152=CARTESIAN_POINT('Ctrl Pts',(10.0502525316942,4.32761534819776,-9.73909094732754));
#10153=CARTESIAN_POINT('Ctrl Pts',(10.0502525316942,4.316044643808,-9.78957710119959));
#10154=CARTESIAN_POINT('Ctrl Pts',(10.0502525316942,4.30693895110861,-9.8275230661634));
#10155=CARTESIAN_POINT('Ctrl Pts',(10.0502525316942,4.30067875926925,-9.85285646666673));
#10156=CARTESIAN_POINT('Ctrl Pts',(10.0502525316942,4.29750123086779,-9.86553218952114));
#10157=CARTESIAN_POINT('',(10.0502525316942,2.63468906623289,-8.77492596468499));
#10158=CARTESIAN_POINT('Ctrl Pts',(10.0502525316942,4.29750123086779,-9.86553218952114));
#10159=CARTESIAN_POINT('Ctrl Pts',(10.0502525316942,4.25997612031891,-9.87375991529634));
#10160=CARTESIAN_POINT('Ctrl Pts',(10.0502525316942,4.18685412967622,-9.88905601939953));
#10161=CARTESIAN_POINT('Ctrl Pts',(10.0502525316942,4.08295585472858,-9.9085221213413));
#10162=CARTESIAN_POINT('Ctrl Pts',(10.0502525316942,3.95601502356553,-9.9275083219784));
#10163=CARTESIAN_POINT('Ctrl Pts',(10.0502525316942,3.81664870098641,-9.93963159251159));
#10164=CARTESIAN_POINT('Ctrl Pts',(10.0502525316942,3.69635378003033,-9.94029010584861));
#10165=CARTESIAN_POINT('Ctrl Pts',(10.0502525316942,3.59449506329372,-9.92986863879505));
#10166=CARTESIAN_POINT('Ctrl Pts',(10.0502525316942,3.50984697030288,-9.90910889595984));
#10167=CARTESIAN_POINT('Ctrl Pts',(10.0502525316942,3.44044633176199,-9.87919842483915));
#10168=CARTESIAN_POINT('Ctrl Pts',(10.0502525316942,3.38330805268968,-9.84194232635164));
#10169=CARTESIAN_POINT('Ctrl Pts',(10.0502525316942,3.3347416451379,-9.79957216249457));
#10170=CARTESIAN_POINT('Ctrl Pts',(10.0502525316942,3.29095547943263,-9.75438117654386));
#10171=CARTESIAN_POINT('Ctrl Pts',(10.0502525316942,3.24858483776411,-9.70840543702524));
#10172=CARTESIAN_POINT('Ctrl Pts',(10.0502525316942,3.20521277465607,-9.66310949495059));
#10173=CARTESIAN_POINT('Ctrl Pts',(10.0502525316942,3.16000321945708,-9.61900380828622));
#10174=CARTESIAN_POINT('Ctrl Pts',(10.0502525316942,3.11336354092674,-9.57585180276088));
#10175=CARTESIAN_POINT('Ctrl Pts',(10.0502525316942,3.06641977252332,-9.53299079371256));
#10176=CARTESIAN_POINT('Ctrl Pts',(10.0502525316942,3.02056794696251,-9.4896066485377));
#10177=CARTESIAN_POINT('Ctrl Pts',(10.0502525316942,2.97698682564639,-9.44503212038191));
#10178=CARTESIAN_POINT('Ctrl Pts',(10.0502525316942,2.9361940142505,-9.39901842603143));
#10179=CARTESIAN_POINT('Ctrl Pts',(10.0502525316942,2.8982483626292,-9.35160551556488));
#10180=CARTESIAN_POINT('Ctrl Pts',(10.0502525316942,2.86292873701901,-9.30300690939252));
#10181=CARTESIAN_POINT('Ctrl Pts',(10.0502525316942,2.82990845462794,-9.25349741301079));
#10182=CARTESIAN_POINT('Ctrl Pts',(10.0502525316942,2.79895351207997,-9.20328535602728));
#10183=CARTESIAN_POINT('Ctrl Pts',(10.0502525316942,2.77003209344587,-9.15244173271444));
#10184=CARTESIAN_POINT('Ctrl Pts',(10.0502525316942,2.74322870228394,-9.10095481538197));
#10185=CARTESIAN_POINT('Ctrl Pts',(10.0502525316942,2.71869695754934,-9.04875963323664));
#10186=CARTESIAN_POINT('Ctrl Pts',(10.0502525316942,2.69660154669561,-8.99577459934956));
#10187=CARTESIAN_POINT('Ctrl Pts',(10.0502525316942,2.67705351804929,-8.94194140034058));
#10188=CARTESIAN_POINT('Ctrl Pts',(10.0502525316942,2.66010336866474,-8.88723149748883));
#10189=CARTESIAN_POINT('Ctrl Pts',(10.0502525316942,2.64863401651716,-8.84275317038967));
#10190=CARTESIAN_POINT('Ctrl Pts',(10.0502525316942,2.64120584766726,-8.8089947353088));
#10191=CARTESIAN_POINT('Ctrl Pts',(10.0502525316942,2.63677452882417,-8.78631177678628));
#10192=CARTESIAN_POINT('Ctrl Pts',(10.0502525316942,2.63468906623289,-8.77492596468499));
#10193=CARTESIAN_POINT('',(10.0502525316942,1.47863151154858,-9.041822881172));
#10194=CARTESIAN_POINT('Origin',(10.0502525316942,0.,0.));
#10195=CARTESIAN_POINT('',(10.0502525316942,1.03854944428814,-10.7106795892491));
#10196=CARTESIAN_POINT('Ctrl Pts',(10.0502525316942,1.47863151154858,-9.041822881172));
#10197=CARTESIAN_POINT('Ctrl Pts',(10.0502525316942,1.48142903122265,-9.05241341063017));
#10198=CARTESIAN_POINT('Ctrl Pts',(10.0502525316942,1.48681431784179,-9.0736287027809));
#10199=CARTESIAN_POINT('Ctrl Pts',(10.0502525316942,1.49426299078246,-9.10555434079238));
#10200=CARTESIAN_POINT('Ctrl Pts',(10.0502525316942,1.50293375169959,-9.14832762892595));
#10201=CARTESIAN_POINT('Ctrl Pts',(10.0502525316942,1.51165206039235,-9.20213819442161));
#10202=CARTESIAN_POINT('Ctrl Pts',(10.0502525316942,1.51821671513724,-9.25629193365179));
#10203=CARTESIAN_POINT('Ctrl Pts',(10.0502525316942,1.52257856936539,-9.31078441132333));
#10204=CARTESIAN_POINT('Ctrl Pts',(10.0502525316942,1.52467115182437,-9.36560546949212));
#10205=CARTESIAN_POINT('Ctrl Pts',(10.0502525316942,1.52441199543777,-9.42073743324162));
#10206=CARTESIAN_POINT('Ctrl Pts',(10.0502525316942,1.52172656066024,-9.47615638983506));
#10207=CARTESIAN_POINT('Ctrl Pts',(10.0502525316942,1.51657146095807,-9.53183308717807));
#10208=CARTESIAN_POINT('Ctrl Pts',(10.0502525316942,1.50895693238989,-9.58773391775221));
#10209=CARTESIAN_POINT('Ctrl Pts',(10.0502525316942,1.49897455623114,-9.64382166809154));
#10210=CARTESIAN_POINT('Ctrl Pts',(10.0502525316942,1.48681164197681,-9.70005659890418));
#10211=CARTESIAN_POINT('Ctrl Pts',(10.0502525316942,1.472706711821,-9.75639893594512));
#10212=CARTESIAN_POINT('Ctrl Pts',(10.0502525316942,1.45691330418438,-9.81281120439258));
#10213=CARTESIAN_POINT('Ctrl Pts',(10.0502525316942,1.43966301743384,-9.86926046040473));
#10214=CARTESIAN_POINT('Ctrl Pts',(10.0502525316942,1.4211247852801,-9.9257209332579));
#10215=CARTESIAN_POINT('Ctrl Pts',(10.0502525316942,1.40137929597453,-9.98217543513636));
#10216=CARTESIAN_POINT('Ctrl Pts',(10.0502525316942,1.38044913636064,-10.0386123354999));
#10217=CARTESIAN_POINT('Ctrl Pts',(10.0502525316942,1.3583201853205,-10.0950232336429));
#10218=CARTESIAN_POINT('Ctrl Pts',(10.0502525316942,1.33496549883664,-10.1514004985561));
#10219=CARTESIAN_POINT('Ctrl Pts',(10.0502525316942,1.31037031610781,-10.2077346253654));
#10220=CARTESIAN_POINT('Ctrl Pts',(10.0502525316942,1.2845505698718,-10.26401245069));
#10221=CARTESIAN_POINT('Ctrl Pts',(10.0502525316942,1.2575411104082,-10.3202191159745));
#10222=CARTESIAN_POINT('Ctrl Pts',(10.0502525316942,1.22938873407214,-10.3763394931394));
#10223=CARTESIAN_POINT('Ctrl Pts',(10.0502525316942,1.20014382966931,-10.4323597856746));
#10224=CARTESIAN_POINT('Ctrl Pts',(10.0502525316942,1.16985259538408,-10.4882691830915));
#10225=CARTESIAN_POINT('Ctrl Pts',(10.0502525316942,1.13855017696687,-10.5440612301269));
#10226=CARTESIAN_POINT('Ctrl Pts',(10.0502525316942,1.10626216443499,-10.599732595958));
#10227=CARTESIAN_POINT('Ctrl Pts',(10.0502525316942,1.07965669109989,-10.6441722372873));
#10228=CARTESIAN_POINT('Ctrl Pts',(10.0502525316942,1.05927071468098,-10.6774471807436));
#10229=CARTESIAN_POINT('Ctrl Pts',(10.0502525316942,1.04548846715806,-10.6996061707058));
#10230=CARTESIAN_POINT('Ctrl Pts',(10.0502525316942,1.03854944428814,-10.7106795892491));
#10231=CARTESIAN_POINT('',(10.0502525316942,-0.205863042617262,-9.15961421508102));
#10232=CARTESIAN_POINT('Ctrl Pts',(10.0502525316942,1.03854944428814,-10.7106795892491));
#10233=CARTESIAN_POINT('Ctrl Pts',(10.0502525316942,1.00031843628634,-10.7069087245865));
#10234=CARTESIAN_POINT('Ctrl Pts',(10.0502525316942,0.926048534485517,-10.6988602462966));
#10235=CARTESIAN_POINT('Ctrl Pts',(10.0502525316942,0.821220046750494,-10.6852672767501));
#10236=CARTESIAN_POINT('Ctrl Pts',(10.0502525316942,0.694625083433483,-10.6640973524763));
#10237=CARTESIAN_POINT('Ctrl Pts',(10.0502525316942,0.558333537570359,-10.6325607057952));
#10238=CARTESIAN_POINT('Ctrl Pts',(10.0502525316942,0.443722777305704,-10.596013814283));
#10239=CARTESIAN_POINT('Ctrl Pts',(10.0502525316942,0.35006979143776,-10.5546263356355));
#10240=CARTESIAN_POINT('Ctrl Pts',(10.0502525316942,0.275979784341795,-10.5087249476599));
#10241=CARTESIAN_POINT('Ctrl Pts',(10.0502525316942,0.219218698708486,-10.4588324224655));
#10242=CARTESIAN_POINT('Ctrl Pts',(10.0502525316942,0.176389733643621,-10.4057430679645));
#10243=CARTESIAN_POINT('Ctrl Pts',(10.0502525316942,0.143293435954743,-10.3504388022425));
#10244=CARTESIAN_POINT('Ctrl Pts',(10.0502525316942,0.1156151003885,-10.2939289512549));
#10245=CARTESIAN_POINT('Ctrl Pts',(10.0502525316942,0.0895255103702553,
-10.237110176256));
#10246=CARTESIAN_POINT('Ctrl Pts',(10.0502525316942,0.0622734430034751,
-10.1806284708027));
#10247=CARTESIAN_POINT('Ctrl Pts',(10.0502525316942,0.0329060076605428,
-10.1247109492303));
#10248=CARTESIAN_POINT('Ctrl Pts',(10.0502525316942,0.00188374052503669,
-10.0692584999061));
#10249=CARTESIAN_POINT('Ctrl Pts',(10.0502525316942,-0.0295176561224928,
-10.0139888357391));
#10250=CARTESIAN_POINT('Ctrl Pts',(10.0502525316942,-0.05971889546067,-9.95855906844526));
#10251=CARTESIAN_POINT('Ctrl Pts',(10.0502525316942,-0.0873927181594365,
-9.90269886586131));
#10252=CARTESIAN_POINT('Ctrl Pts',(10.0502525316942,-0.111969973727219,
-9.84633157004081));
#10253=CARTESIAN_POINT('Ctrl Pts',(10.0502525316942,-0.133407037879776,
-9.78951336137147));
#10254=CARTESIAN_POINT('Ctrl Pts',(10.0502525316942,-0.151980202759258,
-9.73237897573987));
#10255=CARTESIAN_POINT('Ctrl Pts',(10.0502525316942,-0.168085081732297,
-9.67508881816964));
#10256=CARTESIAN_POINT('Ctrl Pts',(10.0502525316942,-0.182008602623654,
-9.61776871087166));
#10257=CARTESIAN_POINT('Ctrl Pts',(10.0502525316942,-0.193802962616849,
-9.56047634174856));
#10258=CARTESIAN_POINT('Ctrl Pts',(10.0502525316942,-0.203384169996506,
-9.50322667013965));
#10259=CARTESIAN_POINT('Ctrl Pts',(10.0502525316942,-0.210586047375027,
-9.44600537601646));
#10260=CARTESIAN_POINT('Ctrl Pts',(10.0502525316942,-0.215226755929045,
-9.38878575682053));
#10261=CARTESIAN_POINT('Ctrl Pts',(10.0502525316942,-0.21718266259851,-9.33154666905179));
#10262=CARTESIAN_POINT('Ctrl Pts',(10.0502525316942,-0.216396922881075,
-9.27427657522174));
#10263=CARTESIAN_POINT('Ctrl Pts',(10.0502525316942,-0.2135603660237,-9.2284309476721));
#10264=CARTESIAN_POINT('Ctrl Pts',(10.0502525316942,-0.210193044269049,
-9.1940293375968));
#10265=CARTESIAN_POINT('Ctrl Pts',(10.0502525316942,-0.207398059264384,
-9.1710872092551));
#10266=CARTESIAN_POINT('Ctrl Pts',(10.0502525316942,-0.205863042617262,
-9.15961421508102));
#10267=CARTESIAN_POINT('',(10.0502525316942,-1.38781479615277,-9.05620683581208));
#10268=CARTESIAN_POINT('Origin',(10.0502525316942,0.,0.));
#10269=CARTESIAN_POINT('',(10.0502525316942,-2.32206279789789,-10.5073910450885));
#10270=CARTESIAN_POINT('Ctrl Pts',(10.0502525316942,-1.38781479615277,-9.05620683581208));
#10271=CARTESIAN_POINT('Ctrl Pts',(10.0502525316942,-1.38842685041928,-9.06714350898568));
#10272=CARTESIAN_POINT('Ctrl Pts',(10.0502525316942,-1.38986102430324,-9.08898459591562));
#10273=CARTESIAN_POINT('Ctrl Pts',(10.0502525316942,-1.39264248006707,-9.12164944850753));
#10274=CARTESIAN_POINT('Ctrl Pts',(10.0502525316942,-1.39761376933417,-9.16500867538789));
#10275=CARTESIAN_POINT('Ctrl Pts',(10.0502525316942,-1.40595054425593,-9.21887966989633));
#10276=CARTESIAN_POINT('Ctrl Pts',(10.0502525316942,-1.41644161231465,-9.27241152635132));
#10277=CARTESIAN_POINT('Ctrl Pts',(10.0502525316942,-1.42913234409394,-9.32558483941339));
#10278=CARTESIAN_POINT('Ctrl Pts',(10.0502525316942,-1.44408281853422,-9.37836940755697));
#10279=CARTESIAN_POINT('Ctrl Pts',(10.0502525316942,-1.4613660046363,-9.43072293720942));
#10280=CARTESIAN_POINT('Ctrl Pts',(10.0502525316942,-1.48104540427845,-9.48259965202034));
#10281=CARTESIAN_POINT('Ctrl Pts',(10.0502525316942,-1.50315324111201,-9.53395832441854));
#10282=CARTESIAN_POINT('Ctrl Pts',(10.0502525316942,-1.52766939477237,-9.58477015487067));
#10283=CARTESIAN_POINT('Ctrl Pts',(10.0502525316942,-1.55449526669738,-9.63502805143792));
#10284=CARTESIAN_POINT('Ctrl Pts',(10.0502525316942,-1.5834404348547,-9.68475210162498));
#10285=CARTESIAN_POINT('Ctrl Pts',(10.0502525316942,-1.61426576023972,-9.73397818528844));
#10286=CARTESIAN_POINT('Ctrl Pts',(10.0502525316942,-1.64671853312854,-9.78274900943559));
#10287=CARTESIAN_POINT('Ctrl Pts',(10.0502525316942,-1.68056831017818,-9.8311048104422));
#10288=CARTESIAN_POINT('Ctrl Pts',(10.0502525316942,-1.71564646229066,-9.87907328228114));
#10289=CARTESIAN_POINT('Ctrl Pts',(10.0502525316942,-1.75187093905158,-9.92666301240917));
#10290=CARTESIAN_POINT('Ctrl Pts',(10.0502525316942,-1.78921666506164,-9.97386991924375));
#10291=CARTESIAN_POINT('Ctrl Pts',(10.0502525316942,-1.8276944743413,-10.0206816495736));
#10292=CARTESIAN_POINT('Ctrl Pts',(10.0502525316942,-1.86732763406234,-10.0670826197184));
#10293=CARTESIAN_POINT('Ctrl Pts',(10.0502525316942,-1.9081272454134,-10.1130592286672));
#10294=CARTESIAN_POINT('Ctrl Pts',(10.0502525316942,-1.95007408775204,-10.1586038807877));
#10295=CARTESIAN_POINT('Ctrl Pts',(10.0502525316942,-1.99313042494654,-10.2037132140826));
#10296=CARTESIAN_POINT('Ctrl Pts',(10.0502525316942,-2.03724707618484,-10.2483873017624));
#10297=CARTESIAN_POINT('Ctrl Pts',(10.0502525316942,-2.08237185550883,-10.2926285935634));
#10298=CARTESIAN_POINT('Ctrl Pts',(10.0502525316942,-2.12845748520948,-10.3364410841241));
#10299=CARTESIAN_POINT('Ctrl Pts',(10.0502525316942,-2.17546854490588,-10.3798294947586));
#10300=CARTESIAN_POINT('Ctrl Pts',(10.0502525316942,-2.22337966776441,-10.4227985654164));
#10301=CARTESIAN_POINT('Ctrl Pts',(10.0502525316942,-2.26241558094358,-10.4568416324806));
#10302=CARTESIAN_POINT('Ctrl Pts',(10.0502525316942,-2.29208631967267,-10.4821883711236));
#10303=CARTESIAN_POINT('Ctrl Pts',(10.0502525316942,-2.31204152046505,-10.4990038742164));
#10304=CARTESIAN_POINT('Ctrl Pts',(10.0502525316942,-2.32206279789789,-10.5073910450885));
#10305=CARTESIAN_POINT('',(10.0502525316942,-3.02626384252387,-8.64769560732005));
#10306=CARTESIAN_POINT('Ctrl Pts',(10.0502525316942,-2.32206279789789,-10.5073910450885));
#10307=CARTESIAN_POINT('Ctrl Pts',(10.0502525316942,-2.35725738591831,-10.4919907084944));
#10308=CARTESIAN_POINT('Ctrl Pts',(10.0502525316942,-2.42540514342016,-10.4613854889436));
#10309=CARTESIAN_POINT('Ctrl Pts',(10.0502525316942,-2.52090250118004,-10.4160640224759));
#10310=CARTESIAN_POINT('Ctrl Pts',(10.0502525316942,-2.63475959960258,-10.3568102329785));
#10311=CARTESIAN_POINT('Ctrl Pts',(10.0502525316942,-2.75463520264158,-10.284700695789));
#10312=CARTESIAN_POINT('Ctrl Pts',(10.0502525316942,-2.85234290245999,-10.214525863806));
#10313=CARTESIAN_POINT('Ctrl Pts',(10.0502525316942,-2.92862275068379,-10.1462236683382));
#10314=CARTESIAN_POINT('Ctrl Pts',(10.0502525316942,-2.98490222577489,-10.0796737828909));
#10315=CARTESIAN_POINT('Ctrl Pts',(10.0502525316942,-3.02346758796109,-10.0146830316105));
#10316=CARTESIAN_POINT('Ctrl Pts',(10.0502525316942,-3.04779484151101,-9.95095717700994));
#10317=CARTESIAN_POINT('Ctrl Pts',(10.0502525316942,-3.06218133312374,-9.88813237627935));
#10318=CARTESIAN_POINT('Ctrl Pts',(10.0502525316942,-3.07104249021943,-9.82583523819669));
#10319=CARTESIAN_POINT('Ctrl Pts',(10.0502525316942,-3.07829719773955,-9.76373524529424));
#10320=CARTESIAN_POINT('Ctrl Pts',(10.0502525316942,-3.08676164713489,-9.70159659932322));
#10321=CARTESIAN_POINT('Ctrl Pts',(10.0502525316942,-3.09741227343545,-9.6393408394545));
#10322=CARTESIAN_POINT('Ctrl Pts',(10.0502525316942,-3.10978045352404,-9.57701601843134));
#10323=CARTESIAN_POINT('Ctrl Pts',(10.0502525316942,-3.12256569092543,-9.51474787896063));
#10324=CARTESIAN_POINT('Ctrl Pts',(10.0502525316942,-3.13416003631015,-9.45269834137241));
#10325=CARTESIAN_POINT('Ctrl Pts',(10.0502525316942,-3.14321765381094,-9.39102045019014));
#10326=CARTESIAN_POINT('Ctrl Pts',(10.0502525316942,-3.14917356053584,-9.32981717654858));
#10327=CARTESIAN_POINT('Ctrl Pts',(10.0502525316942,-3.15200362801959,-9.26915543181673));
#10328=CARTESIAN_POINT('Ctrl Pts',(10.0502525316942,-3.15201226138312,-9.2090779784702));
#10329=CARTESIAN_POINT('Ctrl Pts',(10.0502525316942,-3.14962527917495,-9.14961511949843));
#10330=CARTESIAN_POINT('Ctrl Pts',(10.0502525316942,-3.14515444717397,-9.09079785336098));
#10331=CARTESIAN_POINT('Ctrl Pts',(10.0502525316942,-3.13866723439399,-9.0326649146968));
#10332=CARTESIAN_POINT('Ctrl Pts',(10.0502525316942,-3.13008838265685,-8.97525648555044));
#10333=CARTESIAN_POINT('Ctrl Pts',(10.0502525316942,-3.11925542274306,-8.91861029840238));
#10334=CARTESIAN_POINT('Ctrl Pts',(10.0502525316942,-3.10598716411038,-8.86275714889703));
#10335=CARTESIAN_POINT('Ctrl Pts',(10.0502525316942,-3.09015949103058,-8.8077151330875));
#10336=CARTESIAN_POINT('Ctrl Pts',(10.0502525316942,-3.07171477588927,-8.75349084408744));
#10337=CARTESIAN_POINT('Ctrl Pts',(10.0502525316942,-3.0548499719756,-8.71076560553715));
#10338=CARTESIAN_POINT('Ctrl Pts',(10.0502525316942,-3.04101677653125,-8.67908828975171));
#10339=CARTESIAN_POINT('Ctrl Pts',(10.0502525316942,-3.0312690802849,-8.65813272696012));
#10340=CARTESIAN_POINT('Ctrl Pts',(10.0502525316942,-3.02626384252387,-8.64769560732005));
#10341=CARTESIAN_POINT('',(10.0502525316942,-4.11841212213242,-8.18410616705958));
#10342=CARTESIAN_POINT('Origin',(10.0502525316942,0.,0.));
#10343=CARTESIAN_POINT('',(10.0502525316942,-5.45537535466284,-9.2755658561365));
#10344=CARTESIAN_POINT('Ctrl Pts',(10.0502525316942,-4.11841212213242,-8.18410616705958));
#10345=CARTESIAN_POINT('Ctrl Pts',(10.0502525316942,-4.12237383820348,-8.19431842617809));
#10346=CARTESIAN_POINT('Ctrl Pts',(10.0502525316942,-4.1304870856583,-8.21464735012275));
#10347=CARTESIAN_POINT('Ctrl Pts',(10.0502525316942,-4.14322640185693,-8.24485395393399));
#10348=CARTESIAN_POINT('Ctrl Pts',(10.0502525316942,-4.16135311687778,-8.28455481633258));
#10349=CARTESIAN_POINT('Ctrl Pts',(10.0502525316942,-4.18592891379899,-8.33321297157003));
#10350=CARTESIAN_POINT('Ctrl Pts',(10.0502525316942,-4.21244876582417,-8.38088287416164));
#10351=CARTESIAN_POINT('Ctrl Pts',(10.0502525316942,-4.24094982636281,-8.42753204825146));
#10352=CARTESIAN_POINT('Ctrl Pts',(10.0502525316942,-4.27147990109805,-8.47311320506822));
#10353=CARTESIAN_POINT('Ctrl Pts',(10.0502525316942,-4.3040953182409,-8.51756357237276));
#10354=CARTESIAN_POINT('Ctrl Pts',(10.0502525316942,-4.33884232599626,-8.56081999110915));
#10355=CARTESIAN_POINT('Ctrl Pts',(10.0502525316942,-4.37573883085758,-8.60283329387128));
#10356=CARTESIAN_POINT('Ctrl Pts',(10.0502525316942,-4.41475679767577,-8.6435823082099));
#10357=CARTESIAN_POINT('Ctrl Pts',(10.0502525316942,-4.45580026211617,-8.68309075792173));
#10358=CARTESIAN_POINT('Ctrl Pts',(10.0502525316942,-4.4986943294444,-8.72143659100306));
#10359=CARTESIAN_POINT('Ctrl Pts',(10.0502525316942,-4.54322265243728,-8.75872782924178));
#10360=CARTESIAN_POINT('Ctrl Pts',(10.0502525316942,-4.58915808705618,-8.79508318101477));
#10361=CARTESIAN_POINT('Ctrl Pts',(10.0502525316942,-4.63629390238203,-8.83061212429863));
#10362=CARTESIAN_POINT('Ctrl Pts',(10.0502525316942,-4.68447828052063,-8.86539310688376));
#10363=CARTESIAN_POINT('Ctrl Pts',(10.0502525316942,-4.73363584056076,-8.89945965089929));
#10364=CARTESIAN_POINT('Ctrl Pts',(10.0502525316942,-4.78374147310216,-8.93281562325407));
#10365=CARTESIAN_POINT('Ctrl Pts',(10.0502525316942,-4.83480166455838,-8.96544592744964));
#10366=CARTESIAN_POINT('Ctrl Pts',(10.0502525316942,-4.88683372770265,-8.99732855257362));
#10367=CARTESIAN_POINT('Ctrl Pts',(10.0502525316942,-4.93984401744929,-9.02844713284016));
#10368=CARTESIAN_POINT('Ctrl Pts',(10.0502525316942,-4.99381190670161,-9.05880038387882));
#10369=CARTESIAN_POINT('Ctrl Pts',(10.0502525316942,-5.04870046735128,-9.08839676934597));
#10370=CARTESIAN_POINT('Ctrl Pts',(10.0502525316942,-5.10446294828982,-9.11725155657582));
#10371=CARTESIAN_POINT('Ctrl Pts',(10.0502525316942,-5.16105047473192,-9.14538320175401));
#10372=CARTESIAN_POINT('Ctrl Pts',(10.0502525316942,-5.21841931731543,-9.17281011362288));
#10373=CARTESIAN_POINT('Ctrl Pts',(10.0502525316942,-5.27653724822262,-9.19954772791879));
#10374=CARTESIAN_POINT('Ctrl Pts',(10.0502525316942,-5.33538160688598,-9.2256083913841));
#10375=CARTESIAN_POINT('Ctrl Pts',(10.0502525316942,-5.38302685274804,-9.24592251158686));
#10376=CARTESIAN_POINT('Ctrl Pts',(10.0502525316942,-5.41907797515233,-9.26085993003723));
#10377=CARTESIAN_POINT('Ctrl Pts',(10.0502525316942,-5.44325277512453,-9.27068592765741));
#10378=CARTESIAN_POINT('Ctrl Pts',(10.0502525316942,-5.45537535466284,-9.2755658561365));
#10379=CARTESIAN_POINT('',(10.0502525316942,-5.55043285230422,-7.28928030147641));
#10380=CARTESIAN_POINT('Ctrl Pts',(10.0502525316942,-5.45537535466284,-9.2755658561365));
#10381=CARTESIAN_POINT('Ctrl Pts',(10.0502525316942,-5.48408843121132,-9.25004353985722));
#10382=CARTESIAN_POINT('Ctrl Pts',(10.0502525316942,-5.53944326709657,-9.19987743117415));
#10383=CARTESIAN_POINT('Ctrl Pts',(10.0502525316942,-5.61626154813455,-9.12726384869626));
#10384=CARTESIAN_POINT('Ctrl Pts',(10.0502525316942,-5.70623565557996,-9.03572636773682));
#10385=CARTESIAN_POINT('Ctrl Pts',(10.0502525316942,-5.79796105654696,-8.93010252395574));
#10386=CARTESIAN_POINT('Ctrl Pts',(10.0502525316942,-5.86920138549131,-8.83316895299322));
#10387=CARTESIAN_POINT('Ctrl Pts',(10.0502525316942,-5.92064129305387,-8.74463793548674));
#10388=CARTESIAN_POINT('Ctrl Pts',(10.0502525316942,-5.95360120899603,-8.6639539190358));
#10389=CARTESIAN_POINT('Ctrl Pts',(10.0502525316942,-5.97019580138365,-8.59022668922188));
#10390=CARTESIAN_POINT('Ctrl Pts',(10.0502525316942,-5.97364002234323,-8.52210226517413));
#10391=CARTESIAN_POINT('Ctrl Pts',(10.0502525316942,-5.96790845784416,-8.45790665865659));
#10392=CARTESIAN_POINT('Ctrl Pts',(10.0502525316942,-5.95708504467347,-8.39592031140414));
#10393=CARTESIAN_POINT('Ctrl Pts',(10.0502525316942,-5.94479472837688,-8.33461788057945));
#10394=CARTESIAN_POINT('Ctrl Pts',(10.0502525316942,-5.93364300051867,-8.27290485770376));
#10395=CARTESIAN_POINT('Ctrl Pts',(10.0502525316942,-5.92453426026728,-8.2104048870761));
#10396=CARTESIAN_POINT('Ctrl Pts',(10.0502525316942,-5.91703766966772,-8.14730848207823));
#10397=CARTESIAN_POINT('Ctrl Pts',(10.0502525316942,-5.90995523970613,-8.08413710664289));
#10398=CARTESIAN_POINT('Ctrl Pts',(10.0502525316942,-5.90180775582857,-8.02154163982398));
#10399=CARTESIAN_POINT('Ctrl Pts',(10.0502525316942,-5.89136254542228,-7.96008352176745));
#10400=CARTESIAN_POINT('Ctrl Pts',(10.0502525316942,-5.87811409765682,-7.90003527315714));
#10401=CARTESIAN_POINT('Ctrl Pts',(10.0502525316942,-5.86206014174823,-7.84146798659238));
#10402=CARTESIAN_POINT('Ctrl Pts',(10.0502525316942,-5.84350339850201,-7.78432826524869));
#10403=CARTESIAN_POINT('Ctrl Pts',(10.0502525316942,-5.82285820956226,-7.72851334381364));
#10404=CARTESIAN_POINT('Ctrl Pts',(10.0502525316942,-5.80043066085532,-7.67395636265026));
#10405=CARTESIAN_POINT('Ctrl Pts',(10.0502525316942,-5.77629688888814,-7.62067331151744));
#10406=CARTESIAN_POINT('Ctrl Pts',(10.0502525316942,-5.75039773581461,-7.56872566186653));
#10407=CARTESIAN_POINT('Ctrl Pts',(10.0502525316942,-5.72259034420254,-7.51819950516883));
#10408=CARTESIAN_POINT('Ctrl Pts',(10.0502525316942,-5.69271190798352,-7.46918012077942));
#10409=CARTESIAN_POINT('Ctrl Pts',(10.0502525316942,-5.66064997807339,-7.42172307293681));
#10410=CARTESIAN_POINT('Ctrl Pts',(10.0502525316942,-5.62635178473812,-7.37585243997691));
#10411=CARTESIAN_POINT('Ctrl Pts',(10.0502525316942,-5.59710957827922,-7.34042983445952));
#10412=CARTESIAN_POINT('Ctrl Pts',(10.0502525316942,-5.5741645986968,-7.31457760934185));
#10413=CARTESIAN_POINT('Ctrl Pts',(10.0502525316942,-5.55841836363355,-7.2976598885924));
#10414=CARTESIAN_POINT('Ctrl Pts',(10.0502525316942,-5.55043285230422,-7.28928030147641));
#10415=CARTESIAN_POINT('',(10.0502525316942,-6.44587057493322,-6.51088816465466));
#10416=CARTESIAN_POINT('Origin',(10.0502525316942,0.,0.));
#10417=CARTESIAN_POINT('',(10.0502525316942,-8.05467776187827,-7.13578365451838));
#10418=CARTESIAN_POINT('Ctrl Pts',(10.0502525316942,-6.44587057493322,-6.51088816465466));
#10419=CARTESIAN_POINT('Ctrl Pts',(10.0502525316942,-6.45279415243689,-6.51937636264257));
#10420=CARTESIAN_POINT('Ctrl Pts',(10.0502525316942,-6.46679229227336,-6.5362031868863));
#10421=CARTESIAN_POINT('Ctrl Pts',(10.0502525316942,-6.48824245587723,-6.56099470907402));
#10422=CARTESIAN_POINT('Ctrl Pts',(10.0502525316942,-6.51775022748935,-6.59315100996711));
#10423=CARTESIAN_POINT('Ctrl Pts',(10.0502525316942,-6.55615939617772,-6.63183332667763));
#10424=CARTESIAN_POINT('Ctrl Pts',(10.0502525316942,-6.59611208427845,-6.66897501320444));
#10425=CARTESIAN_POINT('Ctrl Pts',(10.0502525316942,-6.63763359119236,-6.70453370213821));
#10426=CARTESIAN_POINT('Ctrl Pts',(10.0502525316942,-6.68075476979194,-6.73844964641633));
#10427=CARTESIAN_POINT('Ctrl Pts',(10.0502525316942,-6.72550979370064,-6.77064573971725));
#10428=CARTESIAN_POINT('Ctrl Pts',(10.0502525316942,-6.77192313035347,-6.801047622728));
#10429=CARTESIAN_POINT('Ctrl Pts',(10.0502525316942,-6.81999661627367,-6.82960300105583));
#10430=CARTESIAN_POINT('Ctrl Pts',(10.0502525316942,-6.86969704580336,-6.8563004018424));
#10431=CARTESIAN_POINT('Ctrl Pts',(10.0502525316942,-6.92094048249309,-6.88119204236944));
#10432=CARTESIAN_POINT('Ctrl Pts',(10.0502525316942,-6.97358467882161,-6.90440610103192));
#10433=CARTESIAN_POINT('Ctrl Pts',(10.0502525316942,-7.02745725692073,-6.92611216762375));
#10434=CARTESIAN_POINT('Ctrl Pts',(10.0502525316942,-7.08237887287821,-6.94649333188842));
#10435=CARTESIAN_POINT('Ctrl Pts',(10.0502525316942,-7.13818674446165,-6.96571759693621));
#10436=CARTESIAN_POINT('Ctrl Pts',(10.0502525316942,-7.19476072597386,-6.98390648535874));
#10437=CARTESIAN_POINT('Ctrl Pts',(10.0502525316942,-7.25203948481561,-7.00111517257795));
#10438=CARTESIAN_POINT('Ctrl Pts',(10.0502525316942,-7.31000033546873,-7.01735509547412));
#10439=CARTESIAN_POINT('Ctrl Pts',(10.0502525316942,-7.36864478180451,-7.032609892012));
#10440=CARTESIAN_POINT('Ctrl Pts',(10.0502525316942,-7.42798248750274,-7.0468532786288));
#10441=CARTESIAN_POINT('Ctrl Pts',(10.0502525316942,-7.48801443914016,-7.06006772676068));
#10442=CARTESIAN_POINT('Ctrl Pts',(10.0502525316942,-7.54872062228975,-7.07225838902223));
#10443=CARTESIAN_POINT('Ctrl Pts',(10.0502525316942,-7.6100685316471,-7.08344472624203));
#10444=CARTESIAN_POINT('Ctrl Pts',(10.0502525316942,-7.67201842213158,-7.09365570540476));
#10445=CARTESIAN_POINT('Ctrl Pts',(10.0502525316942,-7.73452951433514,-7.10292398252533));
#10446=CARTESIAN_POINT('Ctrl Pts',(10.0502525316942,-7.79756590777721,-7.11128057847415));
#10447=CARTESIAN_POINT('Ctrl Pts',(10.0502525316942,-7.86110172188657,-7.11875013245223));
#10448=CARTESIAN_POINT('Ctrl Pts',(10.0502525316942,-7.92511922053603,-7.12535138940982));
#10449=CARTESIAN_POINT('Ctrl Pts',(10.0502525316942,-7.97670995045205,-7.12994807512891));
#10450=CARTESIAN_POINT('Ctrl Pts',(10.0502525316942,-8.01561252148766,-7.13301399479354));
#10451=CARTESIAN_POINT('Ctrl Pts',(10.0502525316942,-8.04164052278268,-7.13488864983229));
#10452=CARTESIAN_POINT('Ctrl Pts',(10.0502525316942,-8.05467776187827,-7.13578365451838));
#10453=CARTESIAN_POINT('',(10.0502525316942,-7.53128682236137,-5.21733945232202));
#10454=CARTESIAN_POINT('Ctrl Pts',(10.0502525316942,-8.05467776187827,-7.13578365451838));
#10455=CARTESIAN_POINT('Ctrl Pts',(10.0502525316942,-8.07409869096647,-7.10263766069576));
#10456=CARTESIAN_POINT('Ctrl Pts',(10.0502525316942,-8.11124208821886,-7.03782127112617));
#10457=CARTESIAN_POINT('Ctrl Pts',(10.0502525316942,-8.16186178396251,-6.94502349601963));
#10458=CARTESIAN_POINT('Ctrl Pts',(10.0502525316942,-8.21914560790757,-6.83016265001357));
#10459=CARTESIAN_POINT('Ctrl Pts',(10.0502525316942,-8.27374208546745,-6.70136369739477));
#10460=CARTESIAN_POINT('Ctrl Pts',(10.0502525316942,-8.31154154378012,-6.58715992075444));
#10461=CARTESIAN_POINT('Ctrl Pts',(10.0502525316942,-8.33310621412631,-6.48706611403476));
#10462=CARTESIAN_POINT('Ctrl Pts',(10.0502525316942,-8.33952022470187,-6.40014588026893));
#10463=CARTESIAN_POINT('Ctrl Pts',(10.0502525316942,-8.33251965296669,-6.32489910686351));
#10464=CARTESIAN_POINT('Ctrl Pts',(10.0502525316942,-8.31474369699109,-6.25904460664515));
#10465=CARTESIAN_POINT('Ctrl Pts',(10.0502525316942,-8.28945512184757,-6.19976210758369));
#10466=CARTESIAN_POINT('Ctrl Pts',(10.0502525316942,-8.26000660950279,-6.1441542067148));
#10467=CARTESIAN_POINT('Ctrl Pts',(10.0502525316942,-8.22937433118026,-6.08965004701613));
#10468=CARTESIAN_POINT('Ctrl Pts',(10.0502525316942,-8.19969803488993,-6.03440354789477));
#10469=CARTESIAN_POINT('Ctrl Pts',(10.0502525316942,-8.17172155504672,-5.9777772990961));
#10470=CARTESIAN_POINT('Ctrl Pts',(10.0502525316942,-8.1450940122787,-5.92008562586321));
#10471=CARTESIAN_POINT('Ctrl Pts',(10.0502525316942,-8.11883719254497,-5.86219466883171));
#10472=CARTESIAN_POINT('Ctrl Pts',(10.0502525316942,-8.09174541189394,-5.80518055320261));
#10473=CARTESIAN_POINT('Ctrl Pts',(10.0502525316942,-8.06281982355119,-5.74995815707108));
#10474=CARTESIAN_POINT('Ctrl Pts',(10.0502525316942,-8.03166387167001,-5.69694287444675));
#10475=CARTESIAN_POINT('Ctrl Pts',(10.0502525316942,-7.99829736542789,-5.64620302012031));
#10476=CARTESIAN_POINT('Ctrl Pts',(10.0502525316942,-7.96299170889331,-5.59759426482043));
#10477=CARTESIAN_POINT('Ctrl Pts',(10.0502525316942,-7.92610920815888,-5.5508908343176));
#10478=CARTESIAN_POINT('Ctrl Pts',(10.0502525316942,-7.88792030747535,-5.50593455556538));
#10479=CARTESIAN_POINT('Ctrl Pts',(10.0502525316942,-7.84850235807098,-5.46271710825366));
#10480=CARTESIAN_POINT('Ctrl Pts',(10.0502525316942,-7.80781809321391,-5.42131523598658));
#10481=CARTESIAN_POINT('Ctrl Pts',(10.0502525316942,-7.76575825114004,-5.38185496199325));
#10482=CARTESIAN_POINT('Ctrl Pts',(10.0502525316942,-7.72219434684711,-5.34446770160195));
#10483=CARTESIAN_POINT('Ctrl Pts',(10.0502525316942,-7.67703660519485,-5.3092410482218));
#10484=CARTESIAN_POINT('Ctrl Pts',(10.0502525316942,-7.63024227979884,-5.27621420845565));
#10485=CARTESIAN_POINT('Ctrl Pts',(10.0502525316942,-7.59148510170534,-5.25156164740301));
#10486=CARTESIAN_POINT('Ctrl Pts',(10.0502525316942,-7.56167435245346,-5.23406510887067));
#10487=CARTESIAN_POINT('Ctrl Pts',(10.0502525316942,-7.54147092977177,-5.22284125454301));
#10488=CARTESIAN_POINT('Ctrl Pts',(10.0502525316942,-7.53128682236137,-5.21733945232202));
#10489=CARTESIAN_POINT('',(10.0502525316942,-8.14236230483842,-4.20033906466803));
#10490=CARTESIAN_POINT('Origin',(10.0502525316942,0.,0.));
#10491=CARTESIAN_POINT('',(10.0502525316942,-9.86553218952113,-4.29750123086779));
#10492=CARTESIAN_POINT('Ctrl Pts',(10.0502525316942,-8.14236230483842,-4.20033906466803));
#10493=CARTESIAN_POINT('Ctrl Pts',(10.0502525316942,-8.15157001576925,-4.20627231756552));
#10494=CARTESIAN_POINT('Ctrl Pts',(10.0502525316942,-8.17008281252941,-4.21794991531197));
#10495=CARTESIAN_POINT('Ctrl Pts',(10.0502525316942,-8.1981441320729,-4.23489958895176));
#10496=CARTESIAN_POINT('Ctrl Pts',(10.0502525316942,-8.23614453399815,-4.2563636455618));
#10497=CARTESIAN_POINT('Ctrl Pts',(10.0502525316942,-8.28462731741005,-4.28128362907021));
#10498=CARTESIAN_POINT('Ctrl Pts',(10.0502525316942,-8.33410199410829,-4.30426141247364));
#10499=CARTESIAN_POINT('Ctrl Pts',(10.0502525316942,-8.38457953300338,-4.32524888402656));
#10500=CARTESIAN_POINT('Ctrl Pts',(10.0502525316942,-8.43607081406306,-4.34417968683382));
#10501=CARTESIAN_POINT('Ctrl Pts',(10.0502525316942,-8.48858451117083,-4.36096992819547));
#10502=CARTESIAN_POINT('Ctrl Pts',(10.0502525316942,-8.54212091594884,-4.37554132734911));
#10503=CARTESIAN_POINT('Ctrl Pts',(10.0502525316942,-8.59666561517837,-4.38784358185488));
#10504=CARTESIAN_POINT('Ctrl Pts',(10.0502525316942,-8.65218348309394,-4.39787604148868));
#10505=CARTESIAN_POINT('Ctrl Pts',(10.0502525316942,-8.70861082741579,-4.4057143056259));
#10506=CARTESIAN_POINT('Ctrl Pts',(10.0502525316942,-8.76585197201427,-4.41152423606579));
#10507=CARTESIAN_POINT('Ctrl Pts',(10.0502525316942,-8.82379538192297,-4.41552038997767));
#10508=CARTESIAN_POINT('Ctrl Pts',(10.0502525316942,-8.88232706878773,-4.41793231637186));
#10509=CARTESIAN_POINT('Ctrl Pts',(10.0502525316942,-8.94134413332185,-4.41897009817737));
#10510=CARTESIAN_POINT('Ctrl Pts',(10.0502525316942,-9.00076986272314,-4.41878643730905));
#10511=CARTESIAN_POINT('Ctrl Pts',(10.0502525316942,-9.06056297636652,-4.41745276152696));
#10512=CARTESIAN_POINT('Ctrl Pts',(10.0502525316942,-9.12070543323243,-4.41498695816126));
#10513=CARTESIAN_POINT('Ctrl Pts',(10.0502525316942,-9.18119360744053,-4.4113730012699));
#10514=CARTESIAN_POINT('Ctrl Pts',(10.0502525316942,-9.24202856762888,-4.40658290745794));
#10515=CARTESIAN_POINT('Ctrl Pts',(10.0502525316942,-9.3032058354636,-4.40059970120156));
#10516=CARTESIAN_POINT('Ctrl Pts',(10.0502525316942,-9.36470796833893,-4.3934344677265));
#10517=CARTESIAN_POINT('Ctrl Pts',(10.0502525316942,-9.42651006560004,-4.38511576007206));
#10518=CARTESIAN_POINT('Ctrl Pts',(10.0502525316942,-9.48858327871958,-4.37568340938316));
#10519=CARTESIAN_POINT('Ctrl Pts',(10.0502525316942,-9.55089891543934,-4.36518107490567));
#10520=CARTESIAN_POINT('Ctrl Pts',(10.0502525316942,-9.61343241834946,-4.35364935309914));
#10521=CARTESIAN_POINT('Ctrl Pts',(10.0502525316942,-9.67616678749592,-4.34111967477257));
#10522=CARTESIAN_POINT('Ctrl Pts',(10.0502525316942,-9.73909094732754,-4.32761534819777));
#10523=CARTESIAN_POINT('Ctrl Pts',(10.0502525316942,-9.78957710119959,-4.316044643808));
#10524=CARTESIAN_POINT('Ctrl Pts',(10.0502525316942,-9.8275230661634,-4.30693895110861));
#10525=CARTESIAN_POINT('Ctrl Pts',(10.0502525316942,-9.85285646666673,-4.30067875926925));
#10526=CARTESIAN_POINT('Ctrl Pts',(10.0502525316942,-9.86553218952113,-4.29750123086779));
#10527=CARTESIAN_POINT('',(10.0502525316942,-8.77492596468499,-2.63468906623289));
#10528=CARTESIAN_POINT('Ctrl Pts',(10.0502525316942,-9.86553218952113,-4.29750123086779));
#10529=CARTESIAN_POINT('Ctrl Pts',(10.0502525316942,-9.87375991529634,-4.25997612031891));
#10530=CARTESIAN_POINT('Ctrl Pts',(10.0502525316942,-9.88905601939953,-4.18685412967622));
#10531=CARTESIAN_POINT('Ctrl Pts',(10.0502525316942,-9.9085221213413,-4.08295585472858));
#10532=CARTESIAN_POINT('Ctrl Pts',(10.0502525316942,-9.9275083219784,-3.95601502356553));
#10533=CARTESIAN_POINT('Ctrl Pts',(10.0502525316942,-9.93963159251159,-3.81664870098641));
#10534=CARTESIAN_POINT('Ctrl Pts',(10.0502525316942,-9.94029010584861,-3.69635378003033));
#10535=CARTESIAN_POINT('Ctrl Pts',(10.0502525316942,-9.92986863879505,-3.59449506329372));
#10536=CARTESIAN_POINT('Ctrl Pts',(10.0502525316942,-9.90910889595984,-3.50984697030288));
#10537=CARTESIAN_POINT('Ctrl Pts',(10.0502525316942,-9.87919842483915,-3.44044633176199));
#10538=CARTESIAN_POINT('Ctrl Pts',(10.0502525316942,-9.84194232635164,-3.38330805268968));
#10539=CARTESIAN_POINT('Ctrl Pts',(10.0502525316942,-9.79957216249457,-3.3347416451379));
#10540=CARTESIAN_POINT('Ctrl Pts',(10.0502525316942,-9.75438117654386,-3.29095547943263));
#10541=CARTESIAN_POINT('Ctrl Pts',(10.0502525316942,-9.70840543702524,-3.24858483776411));
#10542=CARTESIAN_POINT('Ctrl Pts',(10.0502525316942,-9.66310949495059,-3.20521277465607));
#10543=CARTESIAN_POINT('Ctrl Pts',(10.0502525316942,-9.61900380828622,-3.16000321945708));
#10544=CARTESIAN_POINT('Ctrl Pts',(10.0502525316942,-9.57585180276088,-3.11336354092674));
#10545=CARTESIAN_POINT('Ctrl Pts',(10.0502525316942,-9.53299079371256,-3.06641977252332));
#10546=CARTESIAN_POINT('Ctrl Pts',(10.0502525316942,-9.4896066485377,-3.02056794696251));
#10547=CARTESIAN_POINT('Ctrl Pts',(10.0502525316942,-9.44503212038191,-2.97698682564639));
#10548=CARTESIAN_POINT('Ctrl Pts',(10.0502525316942,-9.39901842603143,-2.9361940142505));
#10549=CARTESIAN_POINT('Ctrl Pts',(10.0502525316942,-9.35160551556488,-2.8982483626292));
#10550=CARTESIAN_POINT('Ctrl Pts',(10.0502525316942,-9.30300690939252,-2.86292873701901));
#10551=CARTESIAN_POINT('Ctrl Pts',(10.0502525316942,-9.25349741301079,-2.82990845462794));
#10552=CARTESIAN_POINT('Ctrl Pts',(10.0502525316942,-9.20328535602728,-2.79895351207997));
#10553=CARTESIAN_POINT('Ctrl Pts',(10.0502525316942,-9.15244173271444,-2.77003209344587));
#10554=CARTESIAN_POINT('Ctrl Pts',(10.0502525316942,-9.10095481538197,-2.74322870228394));
#10555=CARTESIAN_POINT('Ctrl Pts',(10.0502525316942,-9.04875963323664,-2.71869695754934));
#10556=CARTESIAN_POINT('Ctrl Pts',(10.0502525316942,-8.99577459934956,-2.69660154669561));
#10557=CARTESIAN_POINT('Ctrl Pts',(10.0502525316942,-8.94194140034058,-2.67705351804929));
#10558=CARTESIAN_POINT('Ctrl Pts',(10.0502525316942,-8.88723149748883,-2.66010336866474));
#10559=CARTESIAN_POINT('Ctrl Pts',(10.0502525316942,-8.84275317038967,-2.64863401651716));
#10560=CARTESIAN_POINT('Ctrl Pts',(10.0502525316942,-8.8089947353088,-2.64120584766726));
#10561=CARTESIAN_POINT('Ctrl Pts',(10.0502525316942,-8.78631177678628,-2.63677452882418));
#10562=CARTESIAN_POINT('Ctrl Pts',(10.0502525316942,-8.77492596468499,-2.63468906623289));
#10563=CARTESIAN_POINT('',(10.0502525316942,-9.041822881172,-1.47863151154858));
#10564=CARTESIAN_POINT('Origin',(10.0502525316942,0.,0.));
#10565=CARTESIAN_POINT('',(10.0502525316942,-10.7106795892491,-1.03854944428814));
#10566=CARTESIAN_POINT('Ctrl Pts',(10.0502525316942,-9.041822881172,-1.47863151154858));
#10567=CARTESIAN_POINT('Ctrl Pts',(10.0502525316942,-9.05241341063017,-1.48142903122265));
#10568=CARTESIAN_POINT('Ctrl Pts',(10.0502525316942,-9.0736287027809,-1.48681431784179));
#10569=CARTESIAN_POINT('Ctrl Pts',(10.0502525316942,-9.10555434079238,-1.49426299078246));
#10570=CARTESIAN_POINT('Ctrl Pts',(10.0502525316942,-9.14832762892595,-1.50293375169959));
#10571=CARTESIAN_POINT('Ctrl Pts',(10.0502525316942,-9.20213819442161,-1.51165206039235));
#10572=CARTESIAN_POINT('Ctrl Pts',(10.0502525316942,-9.25629193365179,-1.51821671513724));
#10573=CARTESIAN_POINT('Ctrl Pts',(10.0502525316942,-9.31078441132333,-1.52257856936539));
#10574=CARTESIAN_POINT('Ctrl Pts',(10.0502525316942,-9.36560546949212,-1.52467115182437));
#10575=CARTESIAN_POINT('Ctrl Pts',(10.0502525316942,-9.42073743324162,-1.52441199543777));
#10576=CARTESIAN_POINT('Ctrl Pts',(10.0502525316942,-9.47615638983506,-1.52172656066024));
#10577=CARTESIAN_POINT('Ctrl Pts',(10.0502525316942,-9.53183308717807,-1.51657146095807));
#10578=CARTESIAN_POINT('Ctrl Pts',(10.0502525316942,-9.58773391775221,-1.50895693238989));
#10579=CARTESIAN_POINT('Ctrl Pts',(10.0502525316942,-9.64382166809154,-1.49897455623114));
#10580=CARTESIAN_POINT('Ctrl Pts',(10.0502525316942,-9.70005659890418,-1.48681164197681));
#10581=CARTESIAN_POINT('Ctrl Pts',(10.0502525316942,-9.75639893594512,-1.472706711821));
#10582=CARTESIAN_POINT('Ctrl Pts',(10.0502525316942,-9.81281120439258,-1.45691330418438));
#10583=CARTESIAN_POINT('Ctrl Pts',(10.0502525316942,-9.86926046040473,-1.43966301743384));
#10584=CARTESIAN_POINT('Ctrl Pts',(10.0502525316942,-9.9257209332579,-1.42112478528011));
#10585=CARTESIAN_POINT('Ctrl Pts',(10.0502525316942,-9.98217543513636,-1.40137929597453));
#10586=CARTESIAN_POINT('Ctrl Pts',(10.0502525316942,-10.0386123354999,-1.38044913636065));
#10587=CARTESIAN_POINT('Ctrl Pts',(10.0502525316942,-10.0950232336429,-1.3583201853205));
#10588=CARTESIAN_POINT('Ctrl Pts',(10.0502525316942,-10.1514004985561,-1.33496549883664));
#10589=CARTESIAN_POINT('Ctrl Pts',(10.0502525316942,-10.2077346253654,-1.31037031610781));
#10590=CARTESIAN_POINT('Ctrl Pts',(10.0502525316942,-10.26401245069,-1.2845505698718));
#10591=CARTESIAN_POINT('Ctrl Pts',(10.0502525316942,-10.3202191159745,-1.2575411104082));
#10592=CARTESIAN_POINT('Ctrl Pts',(10.0502525316942,-10.3763394931394,-1.22938873407215));
#10593=CARTESIAN_POINT('Ctrl Pts',(10.0502525316942,-10.4323597856746,-1.20014382966931));
#10594=CARTESIAN_POINT('Ctrl Pts',(10.0502525316942,-10.4882691830915,-1.16985259538408));
#10595=CARTESIAN_POINT('Ctrl Pts',(10.0502525316942,-10.5440612301269,-1.13855017696687));
#10596=CARTESIAN_POINT('Ctrl Pts',(10.0502525316942,-10.599732595958,-1.10626216443499));
#10597=CARTESIAN_POINT('Ctrl Pts',(10.0502525316942,-10.6441722372873,-1.07965669109989));
#10598=CARTESIAN_POINT('Ctrl Pts',(10.0502525316942,-10.6774471807436,-1.05927071468098));
#10599=CARTESIAN_POINT('Ctrl Pts',(10.0502525316942,-10.6996061707058,-1.04548846715806));
#10600=CARTESIAN_POINT('Ctrl Pts',(10.0502525316942,-10.7106795892491,-1.03854944428814));
#10601=CARTESIAN_POINT('Ctrl Pts',(10.0502525316942,-10.7106795892491,-1.03854944428814));
#10602=CARTESIAN_POINT('Ctrl Pts',(10.0502525316942,-10.7069087245865,-1.00031843628634));
#10603=CARTESIAN_POINT('Ctrl Pts',(10.0502525316942,-10.6988602462966,-0.926048534485518));
#10604=CARTESIAN_POINT('Ctrl Pts',(10.0502525316942,-10.6852672767501,-0.821220046750494));
#10605=CARTESIAN_POINT('Ctrl Pts',(10.0502525316942,-10.6640973524763,-0.694625083433484));
#10606=CARTESIAN_POINT('Ctrl Pts',(10.0502525316942,-10.6325607057952,-0.558333537570359));
#10607=CARTESIAN_POINT('Ctrl Pts',(10.0502525316942,-10.596013814283,-0.443722777305705));
#10608=CARTESIAN_POINT('Ctrl Pts',(10.0502525316942,-10.5546263356355,-0.35006979143776));
#10609=CARTESIAN_POINT('Ctrl Pts',(10.0502525316942,-10.5087249476599,-0.275979784341796));
#10610=CARTESIAN_POINT('Ctrl Pts',(10.0502525316942,-10.4588324224655,-0.219218698708487));
#10611=CARTESIAN_POINT('Ctrl Pts',(10.0502525316942,-10.4057430679645,-0.176389733643621));
#10612=CARTESIAN_POINT('Ctrl Pts',(10.0502525316942,-10.3504388022425,-0.143293435954743));
#10613=CARTESIAN_POINT('Ctrl Pts',(10.0502525316942,-10.2939289512549,-0.1156151003885));
#10614=CARTESIAN_POINT('Ctrl Pts',(10.0502525316942,-10.237110176256,-0.0895255103702559));
#10615=CARTESIAN_POINT('Ctrl Pts',(10.0502525316942,-10.1806284708027,-0.0622734430034757));
#10616=CARTESIAN_POINT('Ctrl Pts',(10.0502525316942,-10.1247109492303,-0.0329060076605434));
#10617=CARTESIAN_POINT('Ctrl Pts',(10.0502525316942,-10.0692584999061,-0.0018837405250373));
#10618=CARTESIAN_POINT('Ctrl Pts',(10.0502525316942,-10.0139888357391,0.0295176561224922));
#10619=CARTESIAN_POINT('Ctrl Pts',(10.0502525316942,-9.95855906844526,0.0597188954606694));
#10620=CARTESIAN_POINT('Ctrl Pts',(10.0502525316942,-9.90269886586131,0.0873927181594359));
#10621=CARTESIAN_POINT('Ctrl Pts',(10.0502525316942,-9.84633157004081,0.111969973727218));
#10622=CARTESIAN_POINT('Ctrl Pts',(10.0502525316942,-9.78951336137147,0.133407037879776));
#10623=CARTESIAN_POINT('Ctrl Pts',(10.0502525316942,-9.73237897573987,0.151980202759258));
#10624=CARTESIAN_POINT('Ctrl Pts',(10.0502525316942,-9.67508881816964,0.168085081732297));
#10625=CARTESIAN_POINT('Ctrl Pts',(10.0502525316942,-9.61776871087166,0.182008602623653));
#10626=CARTESIAN_POINT('Ctrl Pts',(10.0502525316942,-9.56047634174856,0.193802962616848));
#10627=CARTESIAN_POINT('Ctrl Pts',(10.0502525316942,-9.50322667013965,0.203384169996506));
#10628=CARTESIAN_POINT('Ctrl Pts',(10.0502525316942,-9.44600537601646,0.210586047375026));
#10629=CARTESIAN_POINT('Ctrl Pts',(10.0502525316942,-9.38878575682053,0.215226755929044));
#10630=CARTESIAN_POINT('Ctrl Pts',(10.0502525316942,-9.33154666905179,0.21718266259851));
#10631=CARTESIAN_POINT('Ctrl Pts',(10.0502525316942,-9.27427657522174,0.216396922881075));
#10632=CARTESIAN_POINT('Ctrl Pts',(10.0502525316942,-9.2284309476721,0.2135603660237));
#10633=CARTESIAN_POINT('Ctrl Pts',(10.0502525316942,-9.1940293375968,0.210193044269049));
#10634=CARTESIAN_POINT('Ctrl Pts',(10.0502525316942,-9.1710872092551,0.207398059264383));
#10635=CARTESIAN_POINT('Ctrl Pts',(10.0502525316942,-9.15961421508102,0.205863042617261));
#10636=CARTESIAN_POINT('',(10.0502525316942,-10.5073910450885,2.32206279789789));
#10637=CARTESIAN_POINT('Ctrl Pts',(10.0502525316942,-9.05620683581208,1.38781479615277));
#10638=CARTESIAN_POINT('Ctrl Pts',(10.0502525316942,-9.06714350898568,1.38842685041928));
#10639=CARTESIAN_POINT('Ctrl Pts',(10.0502525316942,-9.08898459591562,1.38986102430324));
#10640=CARTESIAN_POINT('Ctrl Pts',(10.0502525316942,-9.12164944850753,1.39264248006707));
#10641=CARTESIAN_POINT('Ctrl Pts',(10.0502525316942,-9.16500867538789,1.39761376933417));
#10642=CARTESIAN_POINT('Ctrl Pts',(10.0502525316942,-9.21887966989633,1.40595054425593));
#10643=CARTESIAN_POINT('Ctrl Pts',(10.0502525316942,-9.27241152635132,1.41644161231465));
#10644=CARTESIAN_POINT('Ctrl Pts',(10.0502525316942,-9.32558483941339,1.42913234409394));
#10645=CARTESIAN_POINT('Ctrl Pts',(10.0502525316942,-9.37836940755697,1.44408281853422));
#10646=CARTESIAN_POINT('Ctrl Pts',(10.0502525316942,-9.43072293720942,1.4613660046363));
#10647=CARTESIAN_POINT('Ctrl Pts',(10.0502525316942,-9.48259965202034,1.48104540427845));
#10648=CARTESIAN_POINT('Ctrl Pts',(10.0502525316942,-9.53395832441854,1.50315324111201));
#10649=CARTESIAN_POINT('Ctrl Pts',(10.0502525316942,-9.58477015487067,1.52766939477237));
#10650=CARTESIAN_POINT('Ctrl Pts',(10.0502525316942,-9.63502805143792,1.55449526669738));
#10651=CARTESIAN_POINT('Ctrl Pts',(10.0502525316942,-9.68475210162498,1.5834404348547));
#10652=CARTESIAN_POINT('Ctrl Pts',(10.0502525316942,-9.73397818528844,1.61426576023972));
#10653=CARTESIAN_POINT('Ctrl Pts',(10.0502525316942,-9.78274900943559,1.64671853312854));
#10654=CARTESIAN_POINT('Ctrl Pts',(10.0502525316942,-9.8311048104422,1.68056831017818));
#10655=CARTESIAN_POINT('Ctrl Pts',(10.0502525316942,-9.87907328228114,1.71564646229066));
#10656=CARTESIAN_POINT('Ctrl Pts',(10.0502525316942,-9.92666301240917,1.75187093905158));
#10657=CARTESIAN_POINT('Ctrl Pts',(10.0502525316942,-9.97386991924375,1.78921666506164));
#10658=CARTESIAN_POINT('Ctrl Pts',(10.0502525316942,-10.0206816495736,1.8276944743413));
#10659=CARTESIAN_POINT('Ctrl Pts',(10.0502525316942,-10.0670826197184,1.86732763406234));
#10660=CARTESIAN_POINT('Ctrl Pts',(10.0502525316942,-10.1130592286672,1.9081272454134));
#10661=CARTESIAN_POINT('Ctrl Pts',(10.0502525316942,-10.1586038807877,1.95007408775204));
#10662=CARTESIAN_POINT('Ctrl Pts',(10.0502525316942,-10.2037132140826,1.99313042494654));
#10663=CARTESIAN_POINT('Ctrl Pts',(10.0502525316942,-10.2483873017624,2.03724707618484));
#10664=CARTESIAN_POINT('Ctrl Pts',(10.0502525316942,-10.2926285935634,2.08237185550883));
#10665=CARTESIAN_POINT('Ctrl Pts',(10.0502525316942,-10.3364410841241,2.12845748520948));
#10666=CARTESIAN_POINT('Ctrl Pts',(10.0502525316942,-10.3798294947586,2.17546854490588));
#10667=CARTESIAN_POINT('Ctrl Pts',(10.0502525316942,-10.4227985654164,2.22337966776441));
#10668=CARTESIAN_POINT('Ctrl Pts',(10.0502525316942,-10.4568416324806,2.26241558094358));
#10669=CARTESIAN_POINT('Ctrl Pts',(10.0502525316942,-10.4821883711236,2.29208631967267));
#10670=CARTESIAN_POINT('Ctrl Pts',(10.0502525316942,-10.4990038742164,2.31204152046505));
#10671=CARTESIAN_POINT('Ctrl Pts',(10.0502525316942,-10.5073910450885,2.32206279789789));
#10672=CARTESIAN_POINT('',(10.0502525316942,-8.64769560732005,3.02626384252387));
#10673=CARTESIAN_POINT('Ctrl Pts',(10.0502525316942,-10.5073910450885,2.32206279789789));
#10674=CARTESIAN_POINT('Ctrl Pts',(10.0502525316942,-10.4919907084944,2.35725738591831));
#10675=CARTESIAN_POINT('Ctrl Pts',(10.0502525316942,-10.4613854889436,2.42540514342016));
#10676=CARTESIAN_POINT('Ctrl Pts',(10.0502525316942,-10.4160640224759,2.52090250118004));
#10677=CARTESIAN_POINT('Ctrl Pts',(10.0502525316942,-10.3568102329785,2.63475959960257));
#10678=CARTESIAN_POINT('Ctrl Pts',(10.0502525316942,-10.284700695789,2.75463520264158));
#10679=CARTESIAN_POINT('Ctrl Pts',(10.0502525316942,-10.214525863806,2.85234290245999));
#10680=CARTESIAN_POINT('Ctrl Pts',(10.0502525316942,-10.1462236683382,2.92862275068379));
#10681=CARTESIAN_POINT('Ctrl Pts',(10.0502525316942,-10.0796737828909,2.98490222577489));
#10682=CARTESIAN_POINT('Ctrl Pts',(10.0502525316942,-10.0146830316105,3.02346758796109));
#10683=CARTESIAN_POINT('Ctrl Pts',(10.0502525316942,-9.95095717700994,3.04779484151101));
#10684=CARTESIAN_POINT('Ctrl Pts',(10.0502525316942,-9.88813237627935,3.06218133312374));
#10685=CARTESIAN_POINT('Ctrl Pts',(10.0502525316942,-9.82583523819669,3.07104249021943));
#10686=CARTESIAN_POINT('Ctrl Pts',(10.0502525316942,-9.76373524529424,3.07829719773955));
#10687=CARTESIAN_POINT('Ctrl Pts',(10.0502525316942,-9.70159659932322,3.08676164713489));
#10688=CARTESIAN_POINT('Ctrl Pts',(10.0502525316942,-9.6393408394545,3.09741227343545));
#10689=CARTESIAN_POINT('Ctrl Pts',(10.0502525316942,-9.57701601843134,3.10978045352404));
#10690=CARTESIAN_POINT('Ctrl Pts',(10.0502525316942,-9.51474787896063,3.12256569092543));
#10691=CARTESIAN_POINT('Ctrl Pts',(10.0502525316942,-9.45269834137241,3.13416003631015));
#10692=CARTESIAN_POINT('Ctrl Pts',(10.0502525316942,-9.39102045019014,3.14321765381094));
#10693=CARTESIAN_POINT('Ctrl Pts',(10.0502525316942,-9.32981717654858,3.14917356053584));
#10694=CARTESIAN_POINT('Ctrl Pts',(10.0502525316942,-9.26915543181673,3.15200362801959));
#10695=CARTESIAN_POINT('Ctrl Pts',(10.0502525316942,-9.2090779784702,3.15201226138312));
#10696=CARTESIAN_POINT('Ctrl Pts',(10.0502525316942,-9.14961511949843,3.14962527917495));
#10697=CARTESIAN_POINT('Ctrl Pts',(10.0502525316942,-9.09079785336098,3.14515444717397));
#10698=CARTESIAN_POINT('Ctrl Pts',(10.0502525316942,-9.0326649146968,3.13866723439399));
#10699=CARTESIAN_POINT('Ctrl Pts',(10.0502525316942,-8.97525648555044,3.13008838265685));
#10700=CARTESIAN_POINT('Ctrl Pts',(10.0502525316942,-8.91861029840238,3.11925542274306));
#10701=CARTESIAN_POINT('Ctrl Pts',(10.0502525316942,-8.86275714889703,3.10598716411038));
#10702=CARTESIAN_POINT('Ctrl Pts',(10.0502525316942,-8.8077151330875,3.09015949103058));
#10703=CARTESIAN_POINT('Ctrl Pts',(10.0502525316942,-8.75349084408744,3.07171477588927));
#10704=CARTESIAN_POINT('Ctrl Pts',(10.0502525316942,-8.71076560553715,3.0548499719756));
#10705=CARTESIAN_POINT('Ctrl Pts',(10.0502525316942,-8.67908828975171,3.04101677653125));
#10706=CARTESIAN_POINT('Ctrl Pts',(10.0502525316942,-8.65813272696012,3.0312690802849));
#10707=CARTESIAN_POINT('Ctrl Pts',(10.0502525316942,-8.64769560732005,3.02626384252387));
#10708=CARTESIAN_POINT('',(10.0502525316942,-8.18410616705958,4.11841212213242));
#10709=CARTESIAN_POINT('Origin',(10.0502525316942,0.,0.));
#10710=CARTESIAN_POINT('',(10.0502525316942,-9.2755658561365,5.45537535466284));
#10711=CARTESIAN_POINT('Ctrl Pts',(10.0502525316942,-8.18410616705958,4.11841212213242));
#10712=CARTESIAN_POINT('Ctrl Pts',(10.0502525316942,-8.19431842617809,4.12237383820348));
#10713=CARTESIAN_POINT('Ctrl Pts',(10.0502525316942,-8.21464735012275,4.1304870856583));
#10714=CARTESIAN_POINT('Ctrl Pts',(10.0502525316942,-8.24485395393399,4.14322640185693));
#10715=CARTESIAN_POINT('Ctrl Pts',(10.0502525316942,-8.28455481633258,4.16135311687778));
#10716=CARTESIAN_POINT('Ctrl Pts',(10.0502525316942,-8.33321297157003,4.18592891379899));
#10717=CARTESIAN_POINT('Ctrl Pts',(10.0502525316942,-8.38088287416164,4.21244876582417));
#10718=CARTESIAN_POINT('Ctrl Pts',(10.0502525316942,-8.42753204825146,4.24094982636281));
#10719=CARTESIAN_POINT('Ctrl Pts',(10.0502525316942,-8.47311320506822,4.27147990109805));
#10720=CARTESIAN_POINT('Ctrl Pts',(10.0502525316942,-8.51756357237276,4.3040953182409));
#10721=CARTESIAN_POINT('Ctrl Pts',(10.0502525316942,-8.56081999110915,4.33884232599626));
#10722=CARTESIAN_POINT('Ctrl Pts',(10.0502525316942,-8.60283329387128,4.37573883085758));
#10723=CARTESIAN_POINT('Ctrl Pts',(10.0502525316942,-8.6435823082099,4.41475679767577));
#10724=CARTESIAN_POINT('Ctrl Pts',(10.0502525316942,-8.68309075792173,4.45580026211617));
#10725=CARTESIAN_POINT('Ctrl Pts',(10.0502525316942,-8.72143659100306,4.4986943294444));
#10726=CARTESIAN_POINT('Ctrl Pts',(10.0502525316942,-8.75872782924178,4.54322265243728));
#10727=CARTESIAN_POINT('Ctrl Pts',(10.0502525316942,-8.79508318101477,4.58915808705618));
#10728=CARTESIAN_POINT('Ctrl Pts',(10.0502525316942,-8.83061212429863,4.63629390238203));
#10729=CARTESIAN_POINT('Ctrl Pts',(10.0502525316942,-8.86539310688376,4.68447828052063));
#10730=CARTESIAN_POINT('Ctrl Pts',(10.0502525316942,-8.89945965089929,4.73363584056076));
#10731=CARTESIAN_POINT('Ctrl Pts',(10.0502525316942,-8.93281562325407,4.78374147310216));
#10732=CARTESIAN_POINT('Ctrl Pts',(10.0502525316942,-8.96544592744964,4.83480166455838));
#10733=CARTESIAN_POINT('Ctrl Pts',(10.0502525316942,-8.99732855257362,4.88683372770265));
#10734=CARTESIAN_POINT('Ctrl Pts',(10.0502525316942,-9.02844713284016,4.93984401744929));
#10735=CARTESIAN_POINT('Ctrl Pts',(10.0502525316942,-9.05880038387882,4.99381190670161));
#10736=CARTESIAN_POINT('Ctrl Pts',(10.0502525316942,-9.08839676934597,5.04870046735128));
#10737=CARTESIAN_POINT('Ctrl Pts',(10.0502525316942,-9.11725155657582,5.10446294828982));
#10738=CARTESIAN_POINT('Ctrl Pts',(10.0502525316942,-9.14538320175401,5.16105047473192));
#10739=CARTESIAN_POINT('Ctrl Pts',(10.0502525316942,-9.17281011362288,5.21841931731543));
#10740=CARTESIAN_POINT('Ctrl Pts',(10.0502525316942,-9.19954772791879,5.27653724822262));
#10741=CARTESIAN_POINT('Ctrl Pts',(10.0502525316942,-9.2256083913841,5.33538160688598));
#10742=CARTESIAN_POINT('Ctrl Pts',(10.0502525316942,-9.24592251158686,5.38302685274804));
#10743=CARTESIAN_POINT('Ctrl Pts',(10.0502525316942,-9.26085993003723,5.41907797515233));
#10744=CARTESIAN_POINT('Ctrl Pts',(10.0502525316942,-9.27068592765741,5.44325277512453));
#10745=CARTESIAN_POINT('Ctrl Pts',(10.0502525316942,-9.2755658561365,5.45537535466284));
#10746=CARTESIAN_POINT('',(10.0502525316942,-7.28928030147641,5.55043285230422));
#10747=CARTESIAN_POINT('Ctrl Pts',(10.0502525316942,-9.2755658561365,5.45537535466284));
#10748=CARTESIAN_POINT('Ctrl Pts',(10.0502525316942,-9.25004353985722,5.48408843121132));
#10749=CARTESIAN_POINT('Ctrl Pts',(10.0502525316942,-9.19987743117415,5.53944326709657));
#10750=CARTESIAN_POINT('Ctrl Pts',(10.0502525316942,-9.12726384869626,5.61626154813455));
#10751=CARTESIAN_POINT('Ctrl Pts',(10.0502525316942,-9.03572636773682,5.70623565557996));
#10752=CARTESIAN_POINT('Ctrl Pts',(10.0502525316942,-8.93010252395574,5.79796105654696));
#10753=CARTESIAN_POINT('Ctrl Pts',(10.0502525316942,-8.83316895299322,5.86920138549131));
#10754=CARTESIAN_POINT('Ctrl Pts',(10.0502525316942,-8.74463793548674,5.92064129305387));
#10755=CARTESIAN_POINT('Ctrl Pts',(10.0502525316942,-8.6639539190358,5.95360120899603));
#10756=CARTESIAN_POINT('Ctrl Pts',(10.0502525316942,-8.59022668922188,5.97019580138365));
#10757=CARTESIAN_POINT('Ctrl Pts',(10.0502525316942,-8.52210226517413,5.97364002234323));
#10758=CARTESIAN_POINT('Ctrl Pts',(10.0502525316942,-8.45790665865659,5.96790845784416));
#10759=CARTESIAN_POINT('Ctrl Pts',(10.0502525316942,-8.39592031140414,5.95708504467347));
#10760=CARTESIAN_POINT('Ctrl Pts',(10.0502525316942,-8.33461788057945,5.94479472837688));
#10761=CARTESIAN_POINT('Ctrl Pts',(10.0502525316942,-8.27290485770376,5.93364300051867));
#10762=CARTESIAN_POINT('Ctrl Pts',(10.0502525316942,-8.2104048870761,5.92453426026728));
#10763=CARTESIAN_POINT('Ctrl Pts',(10.0502525316942,-8.14730848207823,5.91703766966772));
#10764=CARTESIAN_POINT('Ctrl Pts',(10.0502525316942,-8.08413710664289,5.90995523970613));
#10765=CARTESIAN_POINT('Ctrl Pts',(10.0502525316942,-8.02154163982398,5.90180775582857));
#10766=CARTESIAN_POINT('Ctrl Pts',(10.0502525316942,-7.96008352176745,5.89136254542228));
#10767=CARTESIAN_POINT('Ctrl Pts',(10.0502525316942,-7.90003527315714,5.87811409765682));
#10768=CARTESIAN_POINT('Ctrl Pts',(10.0502525316942,-7.84146798659238,5.86206014174823));
#10769=CARTESIAN_POINT('Ctrl Pts',(10.0502525316942,-7.78432826524869,5.84350339850201));
#10770=CARTESIAN_POINT('Ctrl Pts',(10.0502525316942,-7.72851334381364,5.82285820956226));
#10771=CARTESIAN_POINT('Ctrl Pts',(10.0502525316942,-7.67395636265026,5.80043066085532));
#10772=CARTESIAN_POINT('Ctrl Pts',(10.0502525316942,-7.62067331151744,5.77629688888814));
#10773=CARTESIAN_POINT('Ctrl Pts',(10.0502525316942,-7.56872566186653,5.75039773581461));
#10774=CARTESIAN_POINT('Ctrl Pts',(10.0502525316942,-7.51819950516883,5.72259034420254));
#10775=CARTESIAN_POINT('Ctrl Pts',(10.0502525316942,-7.46918012077942,5.69271190798352));
#10776=CARTESIAN_POINT('Ctrl Pts',(10.0502525316942,-7.42172307293681,5.66064997807339));
#10777=CARTESIAN_POINT('Ctrl Pts',(10.0502525316942,-7.37585243997691,5.62635178473812));
#10778=CARTESIAN_POINT('Ctrl Pts',(10.0502525316942,-7.34042983445952,5.59710957827922));
#10779=CARTESIAN_POINT('Ctrl Pts',(10.0502525316942,-7.31457760934185,5.5741645986968));
#10780=CARTESIAN_POINT('Ctrl Pts',(10.0502525316942,-7.2976598885924,5.55841836363355));
#10781=CARTESIAN_POINT('Ctrl Pts',(10.0502525316942,-7.28928030147641,5.55043285230422));
#10782=CARTESIAN_POINT('',(10.0502525316942,-6.51088816465466,6.44587057493322));
#10783=CARTESIAN_POINT('Origin',(10.0502525316942,0.,0.));
#10784=CARTESIAN_POINT('',(10.0502525316942,-7.13578365451838,8.05467776187827));
#10785=CARTESIAN_POINT('Ctrl Pts',(10.0502525316942,-6.51088816465466,6.44587057493322));
#10786=CARTESIAN_POINT('Ctrl Pts',(10.0502525316942,-6.51937636264257,6.45279415243689));
#10787=CARTESIAN_POINT('Ctrl Pts',(10.0502525316942,-6.5362031868863,6.46679229227336));
#10788=CARTESIAN_POINT('Ctrl Pts',(10.0502525316942,-6.56099470907402,6.48824245587723));
#10789=CARTESIAN_POINT('Ctrl Pts',(10.0502525316942,-6.59315100996711,6.51775022748935));
#10790=CARTESIAN_POINT('Ctrl Pts',(10.0502525316942,-6.63183332667763,6.55615939617772));
#10791=CARTESIAN_POINT('Ctrl Pts',(10.0502525316942,-6.66897501320444,6.59611208427845));
#10792=CARTESIAN_POINT('Ctrl Pts',(10.0502525316942,-6.70453370213821,6.63763359119236));
#10793=CARTESIAN_POINT('Ctrl Pts',(10.0502525316942,-6.73844964641633,6.68075476979194));
#10794=CARTESIAN_POINT('Ctrl Pts',(10.0502525316942,-6.77064573971725,6.72550979370064));
#10795=CARTESIAN_POINT('Ctrl Pts',(10.0502525316942,-6.801047622728,6.77192313035347));
#10796=CARTESIAN_POINT('Ctrl Pts',(10.0502525316942,-6.82960300105583,6.81999661627367));
#10797=CARTESIAN_POINT('Ctrl Pts',(10.0502525316942,-6.8563004018424,6.86969704580336));
#10798=CARTESIAN_POINT('Ctrl Pts',(10.0502525316942,-6.88119204236944,6.92094048249309));
#10799=CARTESIAN_POINT('Ctrl Pts',(10.0502525316942,-6.90440610103192,6.97358467882161));
#10800=CARTESIAN_POINT('Ctrl Pts',(10.0502525316942,-6.92611216762375,7.02745725692073));
#10801=CARTESIAN_POINT('Ctrl Pts',(10.0502525316942,-6.94649333188842,7.08237887287821));
#10802=CARTESIAN_POINT('Ctrl Pts',(10.0502525316942,-6.96571759693621,7.13818674446165));
#10803=CARTESIAN_POINT('Ctrl Pts',(10.0502525316942,-6.98390648535874,7.19476072597386));
#10804=CARTESIAN_POINT('Ctrl Pts',(10.0502525316942,-7.00111517257795,7.25203948481561));
#10805=CARTESIAN_POINT('Ctrl Pts',(10.0502525316942,-7.01735509547412,7.31000033546873));
#10806=CARTESIAN_POINT('Ctrl Pts',(10.0502525316942,-7.032609892012,7.36864478180451));
#10807=CARTESIAN_POINT('Ctrl Pts',(10.0502525316942,-7.0468532786288,7.42798248750274));
#10808=CARTESIAN_POINT('Ctrl Pts',(10.0502525316942,-7.06006772676068,7.48801443914016));
#10809=CARTESIAN_POINT('Ctrl Pts',(10.0502525316942,-7.07225838902223,7.54872062228975));
#10810=CARTESIAN_POINT('Ctrl Pts',(10.0502525316942,-7.08344472624203,7.6100685316471));
#10811=CARTESIAN_POINT('Ctrl Pts',(10.0502525316942,-7.09365570540476,7.67201842213158));
#10812=CARTESIAN_POINT('Ctrl Pts',(10.0502525316942,-7.10292398252533,7.73452951433514));
#10813=CARTESIAN_POINT('Ctrl Pts',(10.0502525316942,-7.11128057847415,7.79756590777721));
#10814=CARTESIAN_POINT('Ctrl Pts',(10.0502525316942,-7.11875013245223,7.86110172188657));
#10815=CARTESIAN_POINT('Ctrl Pts',(10.0502525316942,-7.12535138940982,7.92511922053603));
#10816=CARTESIAN_POINT('Ctrl Pts',(10.0502525316942,-7.12994807512891,7.97670995045205));
#10817=CARTESIAN_POINT('Ctrl Pts',(10.0502525316942,-7.13301399479354,8.01561252148766));
#10818=CARTESIAN_POINT('Ctrl Pts',(10.0502525316942,-7.13488864983229,8.04164052278268));
#10819=CARTESIAN_POINT('Ctrl Pts',(10.0502525316942,-7.13578365451838,8.05467776187827));
#10820=CARTESIAN_POINT('',(10.0502525316942,-5.21733945232202,7.53128682236137));
#10821=CARTESIAN_POINT('Ctrl Pts',(10.0502525316942,-7.13578365451838,8.05467776187827));
#10822=CARTESIAN_POINT('Ctrl Pts',(10.0502525316942,-7.10263766069576,8.07409869096647));
#10823=CARTESIAN_POINT('Ctrl Pts',(10.0502525316942,-7.03782127112617,8.11124208821886));
#10824=CARTESIAN_POINT('Ctrl Pts',(10.0502525316942,-6.94502349601963,8.16186178396251));
#10825=CARTESIAN_POINT('Ctrl Pts',(10.0502525316942,-6.83016265001357,8.21914560790757));
#10826=CARTESIAN_POINT('Ctrl Pts',(10.0502525316942,-6.70136369739477,8.27374208546745));
#10827=CARTESIAN_POINT('Ctrl Pts',(10.0502525316942,-6.58715992075444,8.31154154378012));
#10828=CARTESIAN_POINT('Ctrl Pts',(10.0502525316942,-6.48706611403476,8.33310621412631));
#10829=CARTESIAN_POINT('Ctrl Pts',(10.0502525316942,-6.40014588026893,8.33952022470187));
#10830=CARTESIAN_POINT('Ctrl Pts',(10.0502525316942,-6.32489910686351,8.33251965296669));
#10831=CARTESIAN_POINT('Ctrl Pts',(10.0502525316942,-6.25904460664515,8.31474369699109));
#10832=CARTESIAN_POINT('Ctrl Pts',(10.0502525316942,-6.19976210758369,8.28945512184757));
#10833=CARTESIAN_POINT('Ctrl Pts',(10.0502525316942,-6.1441542067148,8.26000660950279));
#10834=CARTESIAN_POINT('Ctrl Pts',(10.0502525316942,-6.08965004701613,8.22937433118026));
#10835=CARTESIAN_POINT('Ctrl Pts',(10.0502525316942,-6.03440354789477,8.19969803488993));
#10836=CARTESIAN_POINT('Ctrl Pts',(10.0502525316942,-5.9777772990961,8.17172155504672));
#10837=CARTESIAN_POINT('Ctrl Pts',(10.0502525316942,-5.92008562586321,8.1450940122787));
#10838=CARTESIAN_POINT('Ctrl Pts',(10.0502525316942,-5.86219466883171,8.11883719254497));
#10839=CARTESIAN_POINT('Ctrl Pts',(10.0502525316942,-5.80518055320261,8.09174541189394));
#10840=CARTESIAN_POINT('Ctrl Pts',(10.0502525316942,-5.74995815707108,8.06281982355119));
#10841=CARTESIAN_POINT('Ctrl Pts',(10.0502525316942,-5.69694287444675,8.03166387167001));
#10842=CARTESIAN_POINT('Ctrl Pts',(10.0502525316942,-5.64620302012031,7.99829736542789));
#10843=CARTESIAN_POINT('Ctrl Pts',(10.0502525316942,-5.59759426482043,7.96299170889331));
#10844=CARTESIAN_POINT('Ctrl Pts',(10.0502525316942,-5.5508908343176,7.92610920815888));
#10845=CARTESIAN_POINT('Ctrl Pts',(10.0502525316942,-5.50593455556538,7.88792030747535));
#10846=CARTESIAN_POINT('Ctrl Pts',(10.0502525316942,-5.46271710825366,7.84850235807098));
#10847=CARTESIAN_POINT('Ctrl Pts',(10.0502525316942,-5.42131523598658,7.80781809321391));
#10848=CARTESIAN_POINT('Ctrl Pts',(10.0502525316942,-5.38185496199325,7.76575825114004));
#10849=CARTESIAN_POINT('Ctrl Pts',(10.0502525316942,-5.34446770160195,7.72219434684711));
#10850=CARTESIAN_POINT('Ctrl Pts',(10.0502525316942,-5.3092410482218,7.67703660519485));
#10851=CARTESIAN_POINT('Ctrl Pts',(10.0502525316942,-5.27621420845565,7.63024227979884));
#10852=CARTESIAN_POINT('Ctrl Pts',(10.0502525316942,-5.25156164740301,7.59148510170534));
#10853=CARTESIAN_POINT('Ctrl Pts',(10.0502525316942,-5.23406510887067,7.56167435245346));
#10854=CARTESIAN_POINT('Ctrl Pts',(10.0502525316942,-5.22284125454301,7.54147092977177));
#10855=CARTESIAN_POINT('Ctrl Pts',(10.0502525316942,-5.21733945232202,7.53128682236137));
#10856=CARTESIAN_POINT('',(10.0502525316942,-4.20033906466803,8.14236230483842));
#10857=CARTESIAN_POINT('Origin',(10.0502525316942,0.,0.));
#10858=CARTESIAN_POINT('',(10.0502525316942,-4.29750123086779,9.86553218952113));
#10859=CARTESIAN_POINT('Ctrl Pts',(10.0502525316942,-4.20033906466803,8.14236230483842));
#10860=CARTESIAN_POINT('Ctrl Pts',(10.0502525316942,-4.20627231756552,8.15157001576925));
#10861=CARTESIAN_POINT('Ctrl Pts',(10.0502525316942,-4.21794991531197,8.17008281252941));
#10862=CARTESIAN_POINT('Ctrl Pts',(10.0502525316942,-4.23489958895176,8.1981441320729));
#10863=CARTESIAN_POINT('Ctrl Pts',(10.0502525316942,-4.2563636455618,8.23614453399815));
#10864=CARTESIAN_POINT('Ctrl Pts',(10.0502525316942,-4.28128362907021,8.28462731741005));
#10865=CARTESIAN_POINT('Ctrl Pts',(10.0502525316942,-4.30426141247364,8.33410199410829));
#10866=CARTESIAN_POINT('Ctrl Pts',(10.0502525316942,-4.32524888402656,8.38457953300338));
#10867=CARTESIAN_POINT('Ctrl Pts',(10.0502525316942,-4.34417968683382,8.43607081406306));
#10868=CARTESIAN_POINT('Ctrl Pts',(10.0502525316942,-4.36096992819547,8.48858451117083));
#10869=CARTESIAN_POINT('Ctrl Pts',(10.0502525316942,-4.37554132734911,8.54212091594884));
#10870=CARTESIAN_POINT('Ctrl Pts',(10.0502525316942,-4.38784358185488,8.59666561517837));
#10871=CARTESIAN_POINT('Ctrl Pts',(10.0502525316942,-4.39787604148868,8.65218348309394));
#10872=CARTESIAN_POINT('Ctrl Pts',(10.0502525316942,-4.4057143056259,8.70861082741579));
#10873=CARTESIAN_POINT('Ctrl Pts',(10.0502525316942,-4.41152423606579,8.76585197201427));
#10874=CARTESIAN_POINT('Ctrl Pts',(10.0502525316942,-4.41552038997767,8.82379538192297));
#10875=CARTESIAN_POINT('Ctrl Pts',(10.0502525316942,-4.41793231637186,8.88232706878773));
#10876=CARTESIAN_POINT('Ctrl Pts',(10.0502525316942,-4.41897009817737,8.94134413332185));
#10877=CARTESIAN_POINT('Ctrl Pts',(10.0502525316942,-4.41878643730905,9.00076986272314));
#10878=CARTESIAN_POINT('Ctrl Pts',(10.0502525316942,-4.41745276152696,9.06056297636652));
#10879=CARTESIAN_POINT('Ctrl Pts',(10.0502525316942,-4.41498695816126,9.12070543323243));
#10880=CARTESIAN_POINT('Ctrl Pts',(10.0502525316942,-4.4113730012699,9.18119360744053));
#10881=CARTESIAN_POINT('Ctrl Pts',(10.0502525316942,-4.40658290745794,9.24202856762888));
#10882=CARTESIAN_POINT('Ctrl Pts',(10.0502525316942,-4.40059970120156,9.3032058354636));
#10883=CARTESIAN_POINT('Ctrl Pts',(10.0502525316942,-4.3934344677265,9.36470796833893));
#10884=CARTESIAN_POINT('Ctrl Pts',(10.0502525316942,-4.38511576007207,9.42651006560004));
#10885=CARTESIAN_POINT('Ctrl Pts',(10.0502525316942,-4.37568340938316,9.48858327871958));
#10886=CARTESIAN_POINT('Ctrl Pts',(10.0502525316942,-4.36518107490567,9.55089891543934));
#10887=CARTESIAN_POINT('Ctrl Pts',(10.0502525316942,-4.35364935309914,9.61343241834946));
#10888=CARTESIAN_POINT('Ctrl Pts',(10.0502525316942,-4.34111967477257,9.67616678749592));
#10889=CARTESIAN_POINT('Ctrl Pts',(10.0502525316942,-4.32761534819777,9.73909094732754));
#10890=CARTESIAN_POINT('Ctrl Pts',(10.0502525316942,-4.316044643808,9.78957710119959));
#10891=CARTESIAN_POINT('Ctrl Pts',(10.0502525316942,-4.30693895110861,9.8275230661634));
#10892=CARTESIAN_POINT('Ctrl Pts',(10.0502525316942,-4.30067875926925,9.85285646666673));
#10893=CARTESIAN_POINT('Ctrl Pts',(10.0502525316942,-4.29750123086779,9.86553218952113));
#10894=CARTESIAN_POINT('',(10.0502525316942,-2.63468906623289,8.77492596468499));
#10895=CARTESIAN_POINT('Ctrl Pts',(10.0502525316942,-4.29750123086779,9.86553218952113));
#10896=CARTESIAN_POINT('Ctrl Pts',(10.0502525316942,-4.25997612031891,9.87375991529634));
#10897=CARTESIAN_POINT('Ctrl Pts',(10.0502525316942,-4.18685412967622,9.88905601939953));
#10898=CARTESIAN_POINT('Ctrl Pts',(10.0502525316942,-4.08295585472858,9.9085221213413));
#10899=CARTESIAN_POINT('Ctrl Pts',(10.0502525316942,-3.95601502356553,9.9275083219784));
#10900=CARTESIAN_POINT('Ctrl Pts',(10.0502525316942,-3.81664870098641,9.93963159251159));
#10901=CARTESIAN_POINT('Ctrl Pts',(10.0502525316942,-3.69635378003033,9.94029010584861));
#10902=CARTESIAN_POINT('Ctrl Pts',(10.0502525316942,-3.59449506329373,9.92986863879505));
#10903=CARTESIAN_POINT('Ctrl Pts',(10.0502525316942,-3.50984697030288,9.90910889595984));
#10904=CARTESIAN_POINT('Ctrl Pts',(10.0502525316942,-3.44044633176199,9.87919842483915));
#10905=CARTESIAN_POINT('Ctrl Pts',(10.0502525316942,-3.38330805268968,9.84194232635164));
#10906=CARTESIAN_POINT('Ctrl Pts',(10.0502525316942,-3.3347416451379,9.79957216249457));
#10907=CARTESIAN_POINT('Ctrl Pts',(10.0502525316942,-3.29095547943264,9.75438117654386));
#10908=CARTESIAN_POINT('Ctrl Pts',(10.0502525316942,-3.24858483776411,9.70840543702524));
#10909=CARTESIAN_POINT('Ctrl Pts',(10.0502525316942,-3.20521277465607,9.66310949495059));
#10910=CARTESIAN_POINT('Ctrl Pts',(10.0502525316942,-3.16000321945708,9.61900380828622));
#10911=CARTESIAN_POINT('Ctrl Pts',(10.0502525316942,-3.11336354092674,9.57585180276088));
#10912=CARTESIAN_POINT('Ctrl Pts',(10.0502525316942,-3.06641977252332,9.53299079371256));
#10913=CARTESIAN_POINT('Ctrl Pts',(10.0502525316942,-3.02056794696251,9.4896066485377));
#10914=CARTESIAN_POINT('Ctrl Pts',(10.0502525316942,-2.97698682564639,9.44503212038191));
#10915=CARTESIAN_POINT('Ctrl Pts',(10.0502525316942,-2.9361940142505,9.39901842603143));
#10916=CARTESIAN_POINT('Ctrl Pts',(10.0502525316942,-2.89824836262921,9.35160551556488));
#10917=CARTESIAN_POINT('Ctrl Pts',(10.0502525316942,-2.86292873701901,9.30300690939252));
#10918=CARTESIAN_POINT('Ctrl Pts',(10.0502525316942,-2.82990845462794,9.25349741301079));
#10919=CARTESIAN_POINT('Ctrl Pts',(10.0502525316942,-2.79895351207997,9.20328535602728));
#10920=CARTESIAN_POINT('Ctrl Pts',(10.0502525316942,-2.77003209344587,9.15244173271444));
#10921=CARTESIAN_POINT('Ctrl Pts',(10.0502525316942,-2.74322870228394,9.10095481538197));
#10922=CARTESIAN_POINT('Ctrl Pts',(10.0502525316942,-2.71869695754934,9.04875963323664));
#10923=CARTESIAN_POINT('Ctrl Pts',(10.0502525316942,-2.69660154669561,8.99577459934956));
#10924=CARTESIAN_POINT('Ctrl Pts',(10.0502525316942,-2.67705351804929,8.94194140034058));
#10925=CARTESIAN_POINT('Ctrl Pts',(10.0502525316942,-2.66010336866474,8.88723149748883));
#10926=CARTESIAN_POINT('Ctrl Pts',(10.0502525316942,-2.64863401651716,8.84275317038967));
#10927=CARTESIAN_POINT('Ctrl Pts',(10.0502525316942,-2.64120584766726,8.8089947353088));
#10928=CARTESIAN_POINT('Ctrl Pts',(10.0502525316942,-2.63677452882418,8.78631177678628));
#10929=CARTESIAN_POINT('Ctrl Pts',(10.0502525316942,-2.63468906623289,8.77492596468499));
#10930=CARTESIAN_POINT('',(10.0502525316942,-1.47863151154858,9.041822881172));
#10931=CARTESIAN_POINT('Origin',(10.0502525316942,0.,0.));
#10932=CARTESIAN_POINT('',(10.0502525316942,-1.03854944428814,10.7106795892491));
#10933=CARTESIAN_POINT('Ctrl Pts',(10.0502525316942,-1.47863151154858,9.041822881172));
#10934=CARTESIAN_POINT('Ctrl Pts',(10.0502525316942,-1.48142903122265,9.05241341063017));
#10935=CARTESIAN_POINT('Ctrl Pts',(10.0502525316942,-1.48681431784179,9.0736287027809));
#10936=CARTESIAN_POINT('Ctrl Pts',(10.0502525316942,-1.49426299078246,9.10555434079238));
#10937=CARTESIAN_POINT('Ctrl Pts',(10.0502525316942,-1.50293375169959,9.14832762892595));
#10938=CARTESIAN_POINT('Ctrl Pts',(10.0502525316942,-1.51165206039235,9.20213819442161));
#10939=CARTESIAN_POINT('Ctrl Pts',(10.0502525316942,-1.51821671513724,9.25629193365179));
#10940=CARTESIAN_POINT('Ctrl Pts',(10.0502525316942,-1.52257856936539,9.31078441132333));
#10941=CARTESIAN_POINT('Ctrl Pts',(10.0502525316942,-1.52467115182437,9.36560546949212));
#10942=CARTESIAN_POINT('Ctrl Pts',(10.0502525316942,-1.52441199543777,9.42073743324162));
#10943=CARTESIAN_POINT('Ctrl Pts',(10.0502525316942,-1.52172656066024,9.47615638983506));
#10944=CARTESIAN_POINT('Ctrl Pts',(10.0502525316942,-1.51657146095807,9.53183308717807));
#10945=CARTESIAN_POINT('Ctrl Pts',(10.0502525316942,-1.50895693238989,9.58773391775221));
#10946=CARTESIAN_POINT('Ctrl Pts',(10.0502525316942,-1.49897455623114,9.64382166809154));
#10947=CARTESIAN_POINT('Ctrl Pts',(10.0502525316942,-1.48681164197681,9.70005659890418));
#10948=CARTESIAN_POINT('Ctrl Pts',(10.0502525316942,-1.472706711821,9.75639893594512));
#10949=CARTESIAN_POINT('Ctrl Pts',(10.0502525316942,-1.45691330418438,9.81281120439258));
#10950=CARTESIAN_POINT('Ctrl Pts',(10.0502525316942,-1.43966301743384,9.86926046040473));
#10951=CARTESIAN_POINT('Ctrl Pts',(10.0502525316942,-1.42112478528011,9.9257209332579));
#10952=CARTESIAN_POINT('Ctrl Pts',(10.0502525316942,-1.40137929597453,9.98217543513636));
#10953=CARTESIAN_POINT('Ctrl Pts',(10.0502525316942,-1.38044913636065,10.0386123354999));
#10954=CARTESIAN_POINT('Ctrl Pts',(10.0502525316942,-1.3583201853205,10.0950232336429));
#10955=CARTESIAN_POINT('Ctrl Pts',(10.0502525316942,-1.33496549883664,10.1514004985561));
#10956=CARTESIAN_POINT('Ctrl Pts',(10.0502525316942,-1.31037031610782,10.2077346253654));
#10957=CARTESIAN_POINT('Ctrl Pts',(10.0502525316942,-1.2845505698718,10.26401245069));
#10958=CARTESIAN_POINT('Ctrl Pts',(10.0502525316942,-1.2575411104082,10.3202191159745));
#10959=CARTESIAN_POINT('Ctrl Pts',(10.0502525316942,-1.22938873407215,10.3763394931394));
#10960=CARTESIAN_POINT('Ctrl Pts',(10.0502525316942,-1.20014382966931,10.4323597856746));
#10961=CARTESIAN_POINT('Ctrl Pts',(10.0502525316942,-1.16985259538408,10.4882691830915));
#10962=CARTESIAN_POINT('Ctrl Pts',(10.0502525316942,-1.13855017696687,10.5440612301269));
#10963=CARTESIAN_POINT('Ctrl Pts',(10.0502525316942,-1.10626216443499,10.599732595958));
#10964=CARTESIAN_POINT('Ctrl Pts',(10.0502525316942,-1.07965669109989,10.6441722372873));
#10965=CARTESIAN_POINT('Ctrl Pts',(10.0502525316942,-1.05927071468098,10.6774471807436));
#10966=CARTESIAN_POINT('Ctrl Pts',(10.0502525316942,-1.04548846715806,10.6996061707058));
#10967=CARTESIAN_POINT('Ctrl Pts',(10.0502525316942,-1.03854944428814,10.7106795892491));
#10968=CARTESIAN_POINT('',(10.0502525316942,0.205863042617261,9.15961421508102));
#10969=CARTESIAN_POINT('Ctrl Pts',(10.0502525316942,-1.03854944428814,10.7106795892491));
#10970=CARTESIAN_POINT('Ctrl Pts',(10.0502525316942,-1.00031843628634,10.7069087245865));
#10971=CARTESIAN_POINT('Ctrl Pts',(10.0502525316942,-0.926048534485518,
10.6988602462966));
#10972=CARTESIAN_POINT('Ctrl Pts',(10.0502525316942,-0.821220046750495,
10.6852672767501));
#10973=CARTESIAN_POINT('Ctrl Pts',(10.0502525316942,-0.694625083433484,
10.6640973524763));
#10974=CARTESIAN_POINT('Ctrl Pts',(10.0502525316942,-0.55833353757036,10.6325607057952));
#10975=CARTESIAN_POINT('Ctrl Pts',(10.0502525316942,-0.443722777305706,
10.596013814283));
#10976=CARTESIAN_POINT('Ctrl Pts',(10.0502525316942,-0.350069791437761,
10.5546263356355));
#10977=CARTESIAN_POINT('Ctrl Pts',(10.0502525316942,-0.275979784341796,
10.5087249476599));
#10978=CARTESIAN_POINT('Ctrl Pts',(10.0502525316942,-0.219218698708488,
10.4588324224655));
#10979=CARTESIAN_POINT('Ctrl Pts',(10.0502525316942,-0.176389733643622,
10.4057430679645));
#10980=CARTESIAN_POINT('Ctrl Pts',(10.0502525316942,-0.143293435954744,
10.3504388022425));
#10981=CARTESIAN_POINT('Ctrl Pts',(10.0502525316942,-0.115615100388501,
10.2939289512549));
#10982=CARTESIAN_POINT('Ctrl Pts',(10.0502525316942,-0.0895255103702565,
10.237110176256));
#10983=CARTESIAN_POINT('Ctrl Pts',(10.0502525316942,-0.0622734430034763,
10.1806284708027));
#10984=CARTESIAN_POINT('Ctrl Pts',(10.0502525316942,-0.032906007660544,
10.1247109492303));
#10985=CARTESIAN_POINT('Ctrl Pts',(10.0502525316942,-0.00188374052503792,
10.0692584999061));
#10986=CARTESIAN_POINT('Ctrl Pts',(10.0502525316942,0.0295176561224916,
10.0139888357391));
#10987=CARTESIAN_POINT('Ctrl Pts',(10.0502525316942,0.0597188954606688,
9.95855906844526));
#10988=CARTESIAN_POINT('Ctrl Pts',(10.0502525316942,0.0873927181594353,
9.90269886586131));
#10989=CARTESIAN_POINT('Ctrl Pts',(10.0502525316942,0.111969973727217,9.84633157004081));
#10990=CARTESIAN_POINT('Ctrl Pts',(10.0502525316942,0.133407037879775,9.78951336137147));
#10991=CARTESIAN_POINT('Ctrl Pts',(10.0502525316942,0.151980202759257,9.73237897573987));
#10992=CARTESIAN_POINT('Ctrl Pts',(10.0502525316942,0.168085081732296,9.67508881816964));
#10993=CARTESIAN_POINT('Ctrl Pts',(10.0502525316942,0.182008602623653,9.61776871087166));
#10994=CARTESIAN_POINT('Ctrl Pts',(10.0502525316942,0.193802962616848,9.56047634174856));
#10995=CARTESIAN_POINT('Ctrl Pts',(10.0502525316942,0.203384169996505,9.50322667013965));
#10996=CARTESIAN_POINT('Ctrl Pts',(10.0502525316942,0.210586047375026,9.44600537601646));
#10997=CARTESIAN_POINT('Ctrl Pts',(10.0502525316942,0.215226755929044,9.38878575682053));
#10998=CARTESIAN_POINT('Ctrl Pts',(10.0502525316942,0.217182662598509,9.33154666905179));
#10999=CARTESIAN_POINT('Ctrl Pts',(10.0502525316942,0.216396922881074,9.27427657522174));
#11000=CARTESIAN_POINT('Ctrl Pts',(10.0502525316942,0.213560366023699,9.2284309476721));
#11001=CARTESIAN_POINT('Ctrl Pts',(10.0502525316942,0.210193044269048,9.1940293375968));
#11002=CARTESIAN_POINT('Ctrl Pts',(10.0502525316942,0.207398059264382,9.1710872092551));
#11003=CARTESIAN_POINT('Ctrl Pts',(10.0502525316942,0.205863042617261,9.15961421508102));
#11004=CARTESIAN_POINT('',(10.0502525316942,1.38781479615277,9.05620683581208));
#11005=CARTESIAN_POINT('Origin',(10.0502525316942,0.,0.));
#11006=CARTESIAN_POINT('',(10.0502525316942,2.32206279789789,10.5073910450885));
#11007=CARTESIAN_POINT('Ctrl Pts',(10.0502525316942,1.38781479615277,9.05620683581208));
#11008=CARTESIAN_POINT('Ctrl Pts',(10.0502525316942,1.38842685041928,9.06714350898568));
#11009=CARTESIAN_POINT('Ctrl Pts',(10.0502525316942,1.38986102430324,9.08898459591562));
#11010=CARTESIAN_POINT('Ctrl Pts',(10.0502525316942,1.39264248006707,9.12164944850753));
#11011=CARTESIAN_POINT('Ctrl Pts',(10.0502525316942,1.39761376933417,9.16500867538789));
#11012=CARTESIAN_POINT('Ctrl Pts',(10.0502525316942,1.40595054425593,9.21887966989634));
#11013=CARTESIAN_POINT('Ctrl Pts',(10.0502525316942,1.41644161231465,9.27241152635132));
#11014=CARTESIAN_POINT('Ctrl Pts',(10.0502525316942,1.42913234409394,9.32558483941339));
#11015=CARTESIAN_POINT('Ctrl Pts',(10.0502525316942,1.44408281853422,9.37836940755697));
#11016=CARTESIAN_POINT('Ctrl Pts',(10.0502525316942,1.4613660046363,9.43072293720942));
#11017=CARTESIAN_POINT('Ctrl Pts',(10.0502525316942,1.48104540427845,9.48259965202034));
#11018=CARTESIAN_POINT('Ctrl Pts',(10.0502525316942,1.50315324111201,9.53395832441854));
#11019=CARTESIAN_POINT('Ctrl Pts',(10.0502525316942,1.52766939477237,9.58477015487067));
#11020=CARTESIAN_POINT('Ctrl Pts',(10.0502525316942,1.55449526669738,9.63502805143792));
#11021=CARTESIAN_POINT('Ctrl Pts',(10.0502525316942,1.5834404348547,9.68475210162498));
#11022=CARTESIAN_POINT('Ctrl Pts',(10.0502525316942,1.61426576023972,9.73397818528844));
#11023=CARTESIAN_POINT('Ctrl Pts',(10.0502525316942,1.64671853312854,9.78274900943559));
#11024=CARTESIAN_POINT('Ctrl Pts',(10.0502525316942,1.68056831017818,9.8311048104422));
#11025=CARTESIAN_POINT('Ctrl Pts',(10.0502525316942,1.71564646229066,9.87907328228115));
#11026=CARTESIAN_POINT('Ctrl Pts',(10.0502525316942,1.75187093905158,9.92666301240917));
#11027=CARTESIAN_POINT('Ctrl Pts',(10.0502525316942,1.78921666506164,9.97386991924375));
#11028=CARTESIAN_POINT('Ctrl Pts',(10.0502525316942,1.8276944743413,10.0206816495737));
#11029=CARTESIAN_POINT('Ctrl Pts',(10.0502525316942,1.86732763406234,10.0670826197184));
#11030=CARTESIAN_POINT('Ctrl Pts',(10.0502525316942,1.9081272454134,10.1130592286672));
#11031=CARTESIAN_POINT('Ctrl Pts',(10.0502525316942,1.95007408775204,10.1586038807877));
#11032=CARTESIAN_POINT('Ctrl Pts',(10.0502525316942,1.99313042494654,10.2037132140826));
#11033=CARTESIAN_POINT('Ctrl Pts',(10.0502525316942,2.03724707618484,10.2483873017624));
#11034=CARTESIAN_POINT('Ctrl Pts',(10.0502525316942,2.08237185550883,10.2926285935634));
#11035=CARTESIAN_POINT('Ctrl Pts',(10.0502525316942,2.12845748520948,10.3364410841241));
#11036=CARTESIAN_POINT('Ctrl Pts',(10.0502525316942,2.17546854490588,10.3798294947586));
#11037=CARTESIAN_POINT('Ctrl Pts',(10.0502525316942,2.22337966776441,10.4227985654164));
#11038=CARTESIAN_POINT('Ctrl Pts',(10.0502525316942,2.26241558094358,10.4568416324806));
#11039=CARTESIAN_POINT('Ctrl Pts',(10.0502525316942,2.29208631967267,10.4821883711236));
#11040=CARTESIAN_POINT('Ctrl Pts',(10.0502525316942,2.31204152046505,10.4990038742164));
#11041=CARTESIAN_POINT('Ctrl Pts',(10.0502525316942,2.32206279789789,10.5073910450885));
#11042=CARTESIAN_POINT('',(10.0502525316942,3.02626384252387,8.64769560732005));
#11043=CARTESIAN_POINT('Ctrl Pts',(10.0502525316942,2.32206279789789,10.5073910450885));
#11044=CARTESIAN_POINT('Ctrl Pts',(10.0502525316942,2.35725738591831,10.4919907084944));
#11045=CARTESIAN_POINT('Ctrl Pts',(10.0502525316942,2.42540514342016,10.4613854889436));
#11046=CARTESIAN_POINT('Ctrl Pts',(10.0502525316942,2.52090250118004,10.4160640224759));
#11047=CARTESIAN_POINT('Ctrl Pts',(10.0502525316942,2.63475959960257,10.3568102329785));
#11048=CARTESIAN_POINT('Ctrl Pts',(10.0502525316942,2.75463520264158,10.284700695789));
#11049=CARTESIAN_POINT('Ctrl Pts',(10.0502525316942,2.85234290245999,10.214525863806));
#11050=CARTESIAN_POINT('Ctrl Pts',(10.0502525316942,2.92862275068379,10.1462236683382));
#11051=CARTESIAN_POINT('Ctrl Pts',(10.0502525316942,2.98490222577489,10.0796737828909));
#11052=CARTESIAN_POINT('Ctrl Pts',(10.0502525316942,3.02346758796109,10.0146830316105));
#11053=CARTESIAN_POINT('Ctrl Pts',(10.0502525316942,3.04779484151101,9.95095717700994));
#11054=CARTESIAN_POINT('Ctrl Pts',(10.0502525316942,3.06218133312374,9.88813237627935));
#11055=CARTESIAN_POINT('Ctrl Pts',(10.0502525316942,3.07104249021943,9.82583523819669));
#11056=CARTESIAN_POINT('Ctrl Pts',(10.0502525316942,3.07829719773955,9.76373524529424));
#11057=CARTESIAN_POINT('Ctrl Pts',(10.0502525316942,3.08676164713489,9.70159659932322));
#11058=CARTESIAN_POINT('Ctrl Pts',(10.0502525316942,3.09741227343545,9.6393408394545));
#11059=CARTESIAN_POINT('Ctrl Pts',(10.0502525316942,3.10978045352404,9.57701601843134));
#11060=CARTESIAN_POINT('Ctrl Pts',(10.0502525316942,3.12256569092543,9.51474787896063));
#11061=CARTESIAN_POINT('Ctrl Pts',(10.0502525316942,3.13416003631015,9.45269834137241));
#11062=CARTESIAN_POINT('Ctrl Pts',(10.0502525316942,3.14321765381094,9.39102045019014));
#11063=CARTESIAN_POINT('Ctrl Pts',(10.0502525316942,3.14917356053584,9.32981717654858));
#11064=CARTESIAN_POINT('Ctrl Pts',(10.0502525316942,3.15200362801959,9.26915543181673));
#11065=CARTESIAN_POINT('Ctrl Pts',(10.0502525316942,3.15201226138312,9.2090779784702));
#11066=CARTESIAN_POINT('Ctrl Pts',(10.0502525316942,3.14962527917495,9.14961511949843));
#11067=CARTESIAN_POINT('Ctrl Pts',(10.0502525316942,3.14515444717397,9.09079785336099));
#11068=CARTESIAN_POINT('Ctrl Pts',(10.0502525316942,3.13866723439399,9.0326649146968));
#11069=CARTESIAN_POINT('Ctrl Pts',(10.0502525316942,3.13008838265685,8.97525648555044));
#11070=CARTESIAN_POINT('Ctrl Pts',(10.0502525316942,3.11925542274306,8.91861029840238));
#11071=CARTESIAN_POINT('Ctrl Pts',(10.0502525316942,3.10598716411038,8.86275714889703));
#11072=CARTESIAN_POINT('Ctrl Pts',(10.0502525316942,3.09015949103058,8.8077151330875));
#11073=CARTESIAN_POINT('Ctrl Pts',(10.0502525316942,3.07171477588927,8.75349084408744));
#11074=CARTESIAN_POINT('Ctrl Pts',(10.0502525316942,3.0548499719756,8.71076560553715));
#11075=CARTESIAN_POINT('Ctrl Pts',(10.0502525316942,3.04101677653125,8.67908828975171));
#11076=CARTESIAN_POINT('Ctrl Pts',(10.0502525316942,3.0312690802849,8.65813272696012));
#11077=CARTESIAN_POINT('Ctrl Pts',(10.0502525316942,3.02626384252387,8.64769560732005));
#11078=CARTESIAN_POINT('',(10.0502525316942,4.11841212213242,8.18410616705958));
#11079=CARTESIAN_POINT('Origin',(10.0502525316942,0.,0.));
#11080=CARTESIAN_POINT('',(10.0502525316942,5.45537535466284,9.2755658561365));
#11081=CARTESIAN_POINT('Ctrl Pts',(10.0502525316942,4.11841212213242,8.18410616705958));
#11082=CARTESIAN_POINT('Ctrl Pts',(10.0502525316942,4.12237383820348,8.19431842617809));
#11083=CARTESIAN_POINT('Ctrl Pts',(10.0502525316942,4.1304870856583,8.21464735012276));
#11084=CARTESIAN_POINT('Ctrl Pts',(10.0502525316942,4.14322640185693,8.24485395393398));
#11085=CARTESIAN_POINT('Ctrl Pts',(10.0502525316942,4.16135311687778,8.28455481633258));
#11086=CARTESIAN_POINT('Ctrl Pts',(10.0502525316942,4.18592891379899,8.33321297157003));
#11087=CARTESIAN_POINT('Ctrl Pts',(10.0502525316942,4.21244876582416,8.38088287416164));
#11088=CARTESIAN_POINT('Ctrl Pts',(10.0502525316942,4.24094982636281,8.42753204825146));
#11089=CARTESIAN_POINT('Ctrl Pts',(10.0502525316942,4.27147990109805,8.47311320506822));
#11090=CARTESIAN_POINT('Ctrl Pts',(10.0502525316942,4.3040953182409,8.51756357237276));
#11091=CARTESIAN_POINT('Ctrl Pts',(10.0502525316942,4.33884232599626,8.56081999110915));
#11092=CARTESIAN_POINT('Ctrl Pts',(10.0502525316942,4.37573883085758,8.60283329387128));
#11093=CARTESIAN_POINT('Ctrl Pts',(10.0502525316942,4.41475679767577,8.6435823082099));
#11094=CARTESIAN_POINT('Ctrl Pts',(10.0502525316942,4.45580026211617,8.68309075792173));
#11095=CARTESIAN_POINT('Ctrl Pts',(10.0502525316942,4.4986943294444,8.72143659100306));
#11096=CARTESIAN_POINT('Ctrl Pts',(10.0502525316942,4.54322265243728,8.75872782924178));
#11097=CARTESIAN_POINT('Ctrl Pts',(10.0502525316942,4.58915808705618,8.79508318101477));
#11098=CARTESIAN_POINT('Ctrl Pts',(10.0502525316942,4.63629390238203,8.83061212429863));
#11099=CARTESIAN_POINT('Ctrl Pts',(10.0502525316942,4.68447828052063,8.86539310688376));
#11100=CARTESIAN_POINT('Ctrl Pts',(10.0502525316942,4.73363584056076,8.89945965089929));
#11101=CARTESIAN_POINT('Ctrl Pts',(10.0502525316942,4.78374147310216,8.93281562325407));
#11102=CARTESIAN_POINT('Ctrl Pts',(10.0502525316942,4.83480166455838,8.96544592744964));
#11103=CARTESIAN_POINT('Ctrl Pts',(10.0502525316942,4.88683372770265,8.99732855257363));
#11104=CARTESIAN_POINT('Ctrl Pts',(10.0502525316942,4.93984401744929,9.02844713284016));
#11105=CARTESIAN_POINT('Ctrl Pts',(10.0502525316942,4.99381190670161,9.05880038387882));
#11106=CARTESIAN_POINT('Ctrl Pts',(10.0502525316942,5.04870046735128,9.08839676934597));
#11107=CARTESIAN_POINT('Ctrl Pts',(10.0502525316942,5.10446294828982,9.11725155657582));
#11108=CARTESIAN_POINT('Ctrl Pts',(10.0502525316942,5.16105047473192,9.14538320175401));
#11109=CARTESIAN_POINT('Ctrl Pts',(10.0502525316942,5.21841931731542,9.17281011362288));
#11110=CARTESIAN_POINT('Ctrl Pts',(10.0502525316942,5.27653724822262,9.19954772791879));
#11111=CARTESIAN_POINT('Ctrl Pts',(10.0502525316942,5.33538160688598,9.22560839138411));
#11112=CARTESIAN_POINT('Ctrl Pts',(10.0502525316942,5.38302685274804,9.24592251158686));
#11113=CARTESIAN_POINT('Ctrl Pts',(10.0502525316942,5.41907797515232,9.26085993003723));
#11114=CARTESIAN_POINT('Ctrl Pts',(10.0502525316942,5.44325277512453,9.27068592765741));
#11115=CARTESIAN_POINT('Ctrl Pts',(10.0502525316942,5.45537535466284,9.2755658561365));
#11116=CARTESIAN_POINT('',(10.0502525316942,5.55043285230422,7.28928030147641));
#11117=CARTESIAN_POINT('Ctrl Pts',(10.0502525316942,5.45537535466284,9.2755658561365));
#11118=CARTESIAN_POINT('Ctrl Pts',(10.0502525316942,5.48408843121132,9.25004353985723));
#11119=CARTESIAN_POINT('Ctrl Pts',(10.0502525316942,5.53944326709657,9.19987743117415));
#11120=CARTESIAN_POINT('Ctrl Pts',(10.0502525316942,5.61626154813455,9.12726384869626));
#11121=CARTESIAN_POINT('Ctrl Pts',(10.0502525316942,5.70623565557996,9.03572636773683));
#11122=CARTESIAN_POINT('Ctrl Pts',(10.0502525316942,5.79796105654696,8.93010252395574));
#11123=CARTESIAN_POINT('Ctrl Pts',(10.0502525316942,5.86920138549131,8.83316895299322));
#11124=CARTESIAN_POINT('Ctrl Pts',(10.0502525316942,5.92064129305387,8.74463793548674));
#11125=CARTESIAN_POINT('Ctrl Pts',(10.0502525316942,5.95360120899603,8.6639539190358));
#11126=CARTESIAN_POINT('Ctrl Pts',(10.0502525316942,5.97019580138365,8.59022668922188));
#11127=CARTESIAN_POINT('Ctrl Pts',(10.0502525316942,5.97364002234322,8.52210226517413));
#11128=CARTESIAN_POINT('Ctrl Pts',(10.0502525316942,5.96790845784416,8.4579066586566));
#11129=CARTESIAN_POINT('Ctrl Pts',(10.0502525316942,5.95708504467347,8.39592031140414));
#11130=CARTESIAN_POINT('Ctrl Pts',(10.0502525316942,5.94479472837688,8.33461788057945));
#11131=CARTESIAN_POINT('Ctrl Pts',(10.0502525316942,5.93364300051867,8.27290485770376));
#11132=CARTESIAN_POINT('Ctrl Pts',(10.0502525316942,5.92453426026728,8.2104048870761));
#11133=CARTESIAN_POINT('Ctrl Pts',(10.0502525316942,5.91703766966772,8.14730848207823));
#11134=CARTESIAN_POINT('Ctrl Pts',(10.0502525316942,5.90995523970613,8.08413710664289));
#11135=CARTESIAN_POINT('Ctrl Pts',(10.0502525316942,5.90180775582857,8.02154163982398));
#11136=CARTESIAN_POINT('Ctrl Pts',(10.0502525316942,5.89136254542228,7.96008352176745));
#11137=CARTESIAN_POINT('Ctrl Pts',(10.0502525316942,5.87811409765682,7.90003527315714));
#11138=CARTESIAN_POINT('Ctrl Pts',(10.0502525316942,5.86206014174823,7.84146798659238));
#11139=CARTESIAN_POINT('Ctrl Pts',(10.0502525316942,5.84350339850201,7.78432826524869));
#11140=CARTESIAN_POINT('Ctrl Pts',(10.0502525316942,5.82285820956226,7.72851334381365));
#11141=CARTESIAN_POINT('Ctrl Pts',(10.0502525316942,5.80043066085532,7.67395636265026));
#11142=CARTESIAN_POINT('Ctrl Pts',(10.0502525316942,5.77629688888814,7.62067331151744));
#11143=CARTESIAN_POINT('Ctrl Pts',(10.0502525316942,5.75039773581461,7.56872566186653));
#11144=CARTESIAN_POINT('Ctrl Pts',(10.0502525316942,5.72259034420254,7.51819950516883));
#11145=CARTESIAN_POINT('Ctrl Pts',(10.0502525316942,5.69271190798352,7.46918012077942));
#11146=CARTESIAN_POINT('Ctrl Pts',(10.0502525316942,5.66064997807339,7.42172307293681));
#11147=CARTESIAN_POINT('Ctrl Pts',(10.0502525316942,5.62635178473812,7.37585243997691));
#11148=CARTESIAN_POINT('Ctrl Pts',(10.0502525316942,5.59710957827922,7.34042983445952));
#11149=CARTESIAN_POINT('Ctrl Pts',(10.0502525316942,5.5741645986968,7.31457760934185));
#11150=CARTESIAN_POINT('Ctrl Pts',(10.0502525316942,5.55841836363355,7.2976598885924));
#11151=CARTESIAN_POINT('Ctrl Pts',(10.0502525316942,5.55043285230422,7.28928030147641));
#11152=CARTESIAN_POINT('',(10.0502525316942,6.44587057493322,6.51088816465466));
#11153=CARTESIAN_POINT('Origin',(10.0502525316942,0.,0.));
#11154=CARTESIAN_POINT('',(10.0502525316942,8.05467776187827,7.13578365451838));
#11155=CARTESIAN_POINT('Ctrl Pts',(10.0502525316942,6.44587057493322,6.51088816465466));
#11156=CARTESIAN_POINT('Ctrl Pts',(10.0502525316942,6.45279415243689,6.51937636264257));
#11157=CARTESIAN_POINT('Ctrl Pts',(10.0502525316942,6.46679229227336,6.5362031868863));
#11158=CARTESIAN_POINT('Ctrl Pts',(10.0502525316942,6.48824245587723,6.56099470907402));
#11159=CARTESIAN_POINT('Ctrl Pts',(10.0502525316942,6.51775022748935,6.59315100996711));
#11160=CARTESIAN_POINT('Ctrl Pts',(10.0502525316942,6.55615939617772,6.63183332667763));
#11161=CARTESIAN_POINT('Ctrl Pts',(10.0502525316942,6.59611208427845,6.66897501320444));
#11162=CARTESIAN_POINT('Ctrl Pts',(10.0502525316942,6.63763359119236,6.70453370213821));
#11163=CARTESIAN_POINT('Ctrl Pts',(10.0502525316942,6.68075476979194,6.73844964641633));
#11164=CARTESIAN_POINT('Ctrl Pts',(10.0502525316942,6.72550979370064,6.77064573971725));
#11165=CARTESIAN_POINT('Ctrl Pts',(10.0502525316942,6.77192313035347,6.801047622728));
#11166=CARTESIAN_POINT('Ctrl Pts',(10.0502525316942,6.81999661627367,6.82960300105583));
#11167=CARTESIAN_POINT('Ctrl Pts',(10.0502525316942,6.86969704580336,6.8563004018424));
#11168=CARTESIAN_POINT('Ctrl Pts',(10.0502525316942,6.92094048249309,6.88119204236944));
#11169=CARTESIAN_POINT('Ctrl Pts',(10.0502525316942,6.97358467882161,6.90440610103192));
#11170=CARTESIAN_POINT('Ctrl Pts',(10.0502525316942,7.02745725692073,6.92611216762375));
#11171=CARTESIAN_POINT('Ctrl Pts',(10.0502525316942,7.08237887287821,6.94649333188842));
#11172=CARTESIAN_POINT('Ctrl Pts',(10.0502525316942,7.13818674446165,6.96571759693621));
#11173=CARTESIAN_POINT('Ctrl Pts',(10.0502525316942,7.19476072597385,6.98390648535874));
#11174=CARTESIAN_POINT('Ctrl Pts',(10.0502525316942,7.25203948481561,7.00111517257795));
#11175=CARTESIAN_POINT('Ctrl Pts',(10.0502525316942,7.31000033546873,7.01735509547412));
#11176=CARTESIAN_POINT('Ctrl Pts',(10.0502525316942,7.36864478180451,7.032609892012));
#11177=CARTESIAN_POINT('Ctrl Pts',(10.0502525316942,7.42798248750274,7.0468532786288));
#11178=CARTESIAN_POINT('Ctrl Pts',(10.0502525316942,7.48801443914016,7.06006772676068));
#11179=CARTESIAN_POINT('Ctrl Pts',(10.0502525316942,7.54872062228975,7.07225838902223));
#11180=CARTESIAN_POINT('Ctrl Pts',(10.0502525316942,7.6100685316471,7.08344472624203));
#11181=CARTESIAN_POINT('Ctrl Pts',(10.0502525316942,7.67201842213158,7.09365570540476));
#11182=CARTESIAN_POINT('Ctrl Pts',(10.0502525316942,7.73452951433514,7.10292398252533));
#11183=CARTESIAN_POINT('Ctrl Pts',(10.0502525316942,7.7975659077772,7.11128057847415));
#11184=CARTESIAN_POINT('Ctrl Pts',(10.0502525316942,7.86110172188656,7.11875013245223));
#11185=CARTESIAN_POINT('Ctrl Pts',(10.0502525316942,7.92511922053603,7.12535138940982));
#11186=CARTESIAN_POINT('Ctrl Pts',(10.0502525316942,7.97670995045205,7.12994807512891));
#11187=CARTESIAN_POINT('Ctrl Pts',(10.0502525316942,8.01561252148766,7.13301399479354));
#11188=CARTESIAN_POINT('Ctrl Pts',(10.0502525316942,8.04164052278268,7.13488864983229));
#11189=CARTESIAN_POINT('Ctrl Pts',(10.0502525316942,8.05467776187827,7.13578365451838));
#11190=CARTESIAN_POINT('',(10.0502525316942,7.53128682236137,5.21733945232202));
#11191=CARTESIAN_POINT('Ctrl Pts',(10.0502525316942,8.05467776187827,7.13578365451838));
#11192=CARTESIAN_POINT('Ctrl Pts',(10.0502525316942,8.07409869096647,7.10263766069576));
#11193=CARTESIAN_POINT('Ctrl Pts',(10.0502525316942,8.11124208821886,7.03782127112617));
#11194=CARTESIAN_POINT('Ctrl Pts',(10.0502525316942,8.1618617839625,6.94502349601963));
#11195=CARTESIAN_POINT('Ctrl Pts',(10.0502525316942,8.21914560790756,6.83016265001357));
#11196=CARTESIAN_POINT('Ctrl Pts',(10.0502525316942,8.27374208546745,6.70136369739477));
#11197=CARTESIAN_POINT('Ctrl Pts',(10.0502525316942,8.31154154378012,6.58715992075444));
#11198=CARTESIAN_POINT('Ctrl Pts',(10.0502525316942,8.33310621412631,6.48706611403476));
#11199=CARTESIAN_POINT('Ctrl Pts',(10.0502525316942,8.33952022470187,6.40014588026893));
#11200=CARTESIAN_POINT('Ctrl Pts',(10.0502525316942,8.33251965296669,6.32489910686351));
#11201=CARTESIAN_POINT('Ctrl Pts',(10.0502525316942,8.31474369699109,6.25904460664515));
#11202=CARTESIAN_POINT('Ctrl Pts',(10.0502525316942,8.28945512184757,6.19976210758369));
#11203=CARTESIAN_POINT('Ctrl Pts',(10.0502525316942,8.26000660950279,6.1441542067148));
#11204=CARTESIAN_POINT('Ctrl Pts',(10.0502525316942,8.22937433118026,6.08965004701613));
#11205=CARTESIAN_POINT('Ctrl Pts',(10.0502525316942,8.19969803488993,6.03440354789477));
#11206=CARTESIAN_POINT('Ctrl Pts',(10.0502525316942,8.17172155504672,5.9777772990961));
#11207=CARTESIAN_POINT('Ctrl Pts',(10.0502525316942,8.1450940122787,5.92008562586321));
#11208=CARTESIAN_POINT('Ctrl Pts',(10.0502525316942,8.11883719254497,5.86219466883171));
#11209=CARTESIAN_POINT('Ctrl Pts',(10.0502525316942,8.09174541189393,5.80518055320261));
#11210=CARTESIAN_POINT('Ctrl Pts',(10.0502525316942,8.06281982355119,5.74995815707108));
#11211=CARTESIAN_POINT('Ctrl Pts',(10.0502525316942,8.03166387167001,5.69694287444675));
#11212=CARTESIAN_POINT('Ctrl Pts',(10.0502525316942,7.99829736542789,5.64620302012031));
#11213=CARTESIAN_POINT('Ctrl Pts',(10.0502525316942,7.96299170889331,5.59759426482043));
#11214=CARTESIAN_POINT('Ctrl Pts',(10.0502525316942,7.92610920815888,5.5508908343176));
#11215=CARTESIAN_POINT('Ctrl Pts',(10.0502525316942,7.88792030747535,5.50593455556538));
#11216=CARTESIAN_POINT('Ctrl Pts',(10.0502525316942,7.84850235807098,5.46271710825366));
#11217=CARTESIAN_POINT('Ctrl Pts',(10.0502525316942,7.80781809321391,5.42131523598658));
#11218=CARTESIAN_POINT('Ctrl Pts',(10.0502525316942,7.76575825114004,5.38185496199325));
#11219=CARTESIAN_POINT('Ctrl Pts',(10.0502525316942,7.72219434684711,5.34446770160195));
#11220=CARTESIAN_POINT('Ctrl Pts',(10.0502525316942,7.67703660519484,5.3092410482218));
#11221=CARTESIAN_POINT('Ctrl Pts',(10.0502525316942,7.63024227979884,5.27621420845565));
#11222=CARTESIAN_POINT('Ctrl Pts',(10.0502525316942,7.59148510170534,5.25156164740301));
#11223=CARTESIAN_POINT('Ctrl Pts',(10.0502525316942,7.56167435245346,5.23406510887067));
#11224=CARTESIAN_POINT('Ctrl Pts',(10.0502525316942,7.54147092977177,5.22284125454301));
#11225=CARTESIAN_POINT('Ctrl Pts',(10.0502525316942,7.53128682236137,5.21733945232202));
#11226=CARTESIAN_POINT('',(10.0502525316942,8.14236230483842,4.20033906466803));
#11227=CARTESIAN_POINT('Origin',(10.0502525316942,0.,0.));
#11228=CARTESIAN_POINT('',(10.0502525316942,9.86553218952113,4.2975012308678));
#11229=CARTESIAN_POINT('Ctrl Pts',(10.0502525316942,8.14236230483842,4.20033906466803));
#11230=CARTESIAN_POINT('Ctrl Pts',(10.0502525316942,8.15157001576925,4.20627231756552));
#11231=CARTESIAN_POINT('Ctrl Pts',(10.0502525316942,8.17008281252941,4.21794991531197));
#11232=CARTESIAN_POINT('Ctrl Pts',(10.0502525316942,8.1981441320729,4.23489958895177));
#11233=CARTESIAN_POINT('Ctrl Pts',(10.0502525316942,8.23614453399815,4.2563636455618));
#11234=CARTESIAN_POINT('Ctrl Pts',(10.0502525316942,8.28462731741005,4.28128362907022));
#11235=CARTESIAN_POINT('Ctrl Pts',(10.0502525316942,8.33410199410829,4.30426141247364));
#11236=CARTESIAN_POINT('Ctrl Pts',(10.0502525316942,8.38457953300338,4.32524888402656));
#11237=CARTESIAN_POINT('Ctrl Pts',(10.0502525316942,8.43607081406306,4.34417968683382));
#11238=CARTESIAN_POINT('Ctrl Pts',(10.0502525316942,8.48858451117083,4.36096992819547));
#11239=CARTESIAN_POINT('Ctrl Pts',(10.0502525316942,8.54212091594884,4.37554132734912));
#11240=CARTESIAN_POINT('Ctrl Pts',(10.0502525316942,8.59666561517837,4.38784358185488));
#11241=CARTESIAN_POINT('Ctrl Pts',(10.0502525316942,8.65218348309394,4.39787604148868));
#11242=CARTESIAN_POINT('Ctrl Pts',(10.0502525316942,8.70861082741579,4.4057143056259));
#11243=CARTESIAN_POINT('Ctrl Pts',(10.0502525316942,8.76585197201427,4.41152423606579));
#11244=CARTESIAN_POINT('Ctrl Pts',(10.0502525316942,8.82379538192297,4.41552038997767));
#11245=CARTESIAN_POINT('Ctrl Pts',(10.0502525316942,8.88232706878773,4.41793231637186));
#11246=CARTESIAN_POINT('Ctrl Pts',(10.0502525316942,8.94134413332185,4.41897009817738));
#11247=CARTESIAN_POINT('Ctrl Pts',(10.0502525316942,9.00076986272314,4.41878643730905));
#11248=CARTESIAN_POINT('Ctrl Pts',(10.0502525316942,9.06056297636652,4.41745276152696));
#11249=CARTESIAN_POINT('Ctrl Pts',(10.0502525316942,9.12070543323243,4.41498695816126));
#11250=CARTESIAN_POINT('Ctrl Pts',(10.0502525316942,9.18119360744053,4.4113730012699));
#11251=CARTESIAN_POINT('Ctrl Pts',(10.0502525316942,9.24202856762888,4.40658290745794));
#11252=CARTESIAN_POINT('Ctrl Pts',(10.0502525316942,9.3032058354636,4.40059970120156));
#11253=CARTESIAN_POINT('Ctrl Pts',(10.0502525316942,9.36470796833893,4.3934344677265));
#11254=CARTESIAN_POINT('Ctrl Pts',(10.0502525316942,9.42651006560004,4.38511576007207));
#11255=CARTESIAN_POINT('Ctrl Pts',(10.0502525316942,9.48858327871958,4.37568340938317));
#11256=CARTESIAN_POINT('Ctrl Pts',(10.0502525316942,9.55089891543934,4.36518107490567));
#11257=CARTESIAN_POINT('Ctrl Pts',(10.0502525316942,9.61343241834946,4.35364935309914));
#11258=CARTESIAN_POINT('Ctrl Pts',(10.0502525316942,9.67616678749592,4.34111967477257));
#11259=CARTESIAN_POINT('Ctrl Pts',(10.0502525316942,9.73909094732754,4.32761534819777));
#11260=CARTESIAN_POINT('Ctrl Pts',(10.0502525316942,9.78957710119959,4.31604464380801));
#11261=CARTESIAN_POINT('Ctrl Pts',(10.0502525316942,9.8275230661634,4.30693895110861));
#11262=CARTESIAN_POINT('Ctrl Pts',(10.0502525316942,9.85285646666673,4.30067875926925));
#11263=CARTESIAN_POINT('Ctrl Pts',(10.0502525316942,9.86553218952113,4.2975012308678));
#11264=CARTESIAN_POINT('',(10.0502525316942,8.77492596468499,2.63468906623289));
#11265=CARTESIAN_POINT('Ctrl Pts',(10.0502525316942,9.86553218952113,4.2975012308678));
#11266=CARTESIAN_POINT('Ctrl Pts',(10.0502525316942,9.87375991529634,4.25997612031891));
#11267=CARTESIAN_POINT('Ctrl Pts',(10.0502525316942,9.88905601939953,4.18685412967622));
#11268=CARTESIAN_POINT('Ctrl Pts',(10.0502525316942,9.9085221213413,4.08295585472858));
#11269=CARTESIAN_POINT('Ctrl Pts',(10.0502525316942,9.9275083219784,3.95601502356554));
#11270=CARTESIAN_POINT('Ctrl Pts',(10.0502525316942,9.93963159251159,3.81664870098642));
#11271=CARTESIAN_POINT('Ctrl Pts',(10.0502525316942,9.94029010584861,3.69635378003033));
#11272=CARTESIAN_POINT('Ctrl Pts',(10.0502525316942,9.92986863879505,3.59449506329373));
#11273=CARTESIAN_POINT('Ctrl Pts',(10.0502525316942,9.90910889595984,3.50984697030289));
#11274=CARTESIAN_POINT('Ctrl Pts',(10.0502525316942,9.87919842483915,3.44044633176199));
#11275=CARTESIAN_POINT('Ctrl Pts',(10.0502525316942,9.84194232635164,3.38330805268968));
#11276=CARTESIAN_POINT('Ctrl Pts',(10.0502525316942,9.79957216249457,3.3347416451379));
#11277=CARTESIAN_POINT('Ctrl Pts',(10.0502525316942,9.75438117654386,3.29095547943264));
#11278=CARTESIAN_POINT('Ctrl Pts',(10.0502525316942,9.70840543702524,3.24858483776411));
#11279=CARTESIAN_POINT('Ctrl Pts',(10.0502525316942,9.66310949495059,3.20521277465607));
#11280=CARTESIAN_POINT('Ctrl Pts',(10.0502525316942,9.61900380828622,3.16000321945709));
#11281=CARTESIAN_POINT('Ctrl Pts',(10.0502525316942,9.57585180276088,3.11336354092674));
#11282=CARTESIAN_POINT('Ctrl Pts',(10.0502525316942,9.53299079371256,3.06641977252332));
#11283=CARTESIAN_POINT('Ctrl Pts',(10.0502525316942,9.4896066485377,3.02056794696251));
#11284=CARTESIAN_POINT('Ctrl Pts',(10.0502525316942,9.44503212038191,2.97698682564639));
#11285=CARTESIAN_POINT('Ctrl Pts',(10.0502525316942,9.39901842603143,2.9361940142505));
#11286=CARTESIAN_POINT('Ctrl Pts',(10.0502525316942,9.35160551556488,2.89824836262921));
#11287=CARTESIAN_POINT('Ctrl Pts',(10.0502525316942,9.30300690939252,2.86292873701902));
#11288=CARTESIAN_POINT('Ctrl Pts',(10.0502525316942,9.25349741301079,2.82990845462794));
#11289=CARTESIAN_POINT('Ctrl Pts',(10.0502525316942,9.20328535602728,2.79895351207997));
#11290=CARTESIAN_POINT('Ctrl Pts',(10.0502525316942,9.15244173271444,2.77003209344587));
#11291=CARTESIAN_POINT('Ctrl Pts',(10.0502525316942,9.10095481538197,2.74322870228394));
#11292=CARTESIAN_POINT('Ctrl Pts',(10.0502525316942,9.04875963323664,2.71869695754935));
#11293=CARTESIAN_POINT('Ctrl Pts',(10.0502525316942,8.99577459934956,2.69660154669561));
#11294=CARTESIAN_POINT('Ctrl Pts',(10.0502525316942,8.94194140034058,2.67705351804929));
#11295=CARTESIAN_POINT('Ctrl Pts',(10.0502525316942,8.88723149748883,2.66010336866474));
#11296=CARTESIAN_POINT('Ctrl Pts',(10.0502525316942,8.84275317038967,2.64863401651716));
#11297=CARTESIAN_POINT('Ctrl Pts',(10.0502525316942,8.8089947353088,2.64120584766726));
#11298=CARTESIAN_POINT('Ctrl Pts',(10.0502525316942,8.78631177678628,2.63677452882418));
#11299=CARTESIAN_POINT('Ctrl Pts',(10.0502525316942,8.77492596468499,2.63468906623289));
#11300=CARTESIAN_POINT('',(10.0502525316942,9.041822881172,1.47863151154858));
#11301=CARTESIAN_POINT('Origin',(10.0502525316942,0.,0.));
#11302=CARTESIAN_POINT('',(10.0502525316942,10.7106795892491,1.03854944428815));
#11303=CARTESIAN_POINT('Ctrl Pts',(10.0502525316942,9.041822881172,1.47863151154858));
#11304=CARTESIAN_POINT('Ctrl Pts',(10.0502525316942,9.05241341063017,1.48142903122266));
#11305=CARTESIAN_POINT('Ctrl Pts',(10.0502525316942,9.0736287027809,1.48681431784179));
#11306=CARTESIAN_POINT('Ctrl Pts',(10.0502525316942,9.10555434079238,1.49426299078246));
#11307=CARTESIAN_POINT('Ctrl Pts',(10.0502525316942,9.14832762892595,1.50293375169959));
#11308=CARTESIAN_POINT('Ctrl Pts',(10.0502525316942,9.20213819442161,1.51165206039235));
#11309=CARTESIAN_POINT('Ctrl Pts',(10.0502525316942,9.25629193365179,1.51821671513724));
#11310=CARTESIAN_POINT('Ctrl Pts',(10.0502525316942,9.31078441132333,1.5225785693654));
#11311=CARTESIAN_POINT('Ctrl Pts',(10.0502525316942,9.36560546949212,1.52467115182437));
#11312=CARTESIAN_POINT('Ctrl Pts',(10.0502525316942,9.42073743324162,1.52441199543777));
#11313=CARTESIAN_POINT('Ctrl Pts',(10.0502525316942,9.47615638983506,1.52172656066024));
#11314=CARTESIAN_POINT('Ctrl Pts',(10.0502525316942,9.53183308717807,1.51657146095807));
#11315=CARTESIAN_POINT('Ctrl Pts',(10.0502525316942,9.58773391775221,1.50895693238989));
#11316=CARTESIAN_POINT('Ctrl Pts',(10.0502525316942,9.64382166809154,1.49897455623114));
#11317=CARTESIAN_POINT('Ctrl Pts',(10.0502525316942,9.70005659890418,1.48681164197681));
#11318=CARTESIAN_POINT('Ctrl Pts',(10.0502525316942,9.75639893594512,1.472706711821));
#11319=CARTESIAN_POINT('Ctrl Pts',(10.0502525316942,9.81281120439258,1.45691330418438));
#11320=CARTESIAN_POINT('Ctrl Pts',(10.0502525316942,9.86926046040473,1.43966301743384));
#11321=CARTESIAN_POINT('Ctrl Pts',(10.0502525316942,9.9257209332579,1.42112478528011));
#11322=CARTESIAN_POINT('Ctrl Pts',(10.0502525316942,9.98217543513636,1.40137929597453));
#11323=CARTESIAN_POINT('Ctrl Pts',(10.0502525316942,10.0386123354999,1.38044913636065));
#11324=CARTESIAN_POINT('Ctrl Pts',(10.0502525316942,10.0950232336429,1.3583201853205));
#11325=CARTESIAN_POINT('Ctrl Pts',(10.0502525316942,10.1514004985561,1.33496549883664));
#11326=CARTESIAN_POINT('Ctrl Pts',(10.0502525316942,10.2077346253654,1.31037031610782));
#11327=CARTESIAN_POINT('Ctrl Pts',(10.0502525316942,10.26401245069,1.2845505698718));
#11328=CARTESIAN_POINT('Ctrl Pts',(10.0502525316942,10.3202191159745,1.2575411104082));
#11329=CARTESIAN_POINT('Ctrl Pts',(10.0502525316942,10.3763394931394,1.22938873407215));
#11330=CARTESIAN_POINT('Ctrl Pts',(10.0502525316942,10.4323597856746,1.20014382966931));
#11331=CARTESIAN_POINT('Ctrl Pts',(10.0502525316942,10.4882691830915,1.16985259538409));
#11332=CARTESIAN_POINT('Ctrl Pts',(10.0502525316942,10.5440612301269,1.13855017696687));
#11333=CARTESIAN_POINT('Ctrl Pts',(10.0502525316942,10.599732595958,1.10626216443499));
#11334=CARTESIAN_POINT('Ctrl Pts',(10.0502525316942,10.6441722372873,1.07965669109989));
#11335=CARTESIAN_POINT('Ctrl Pts',(10.0502525316942,10.6774471807436,1.05927071468098));
#11336=CARTESIAN_POINT('Ctrl Pts',(10.0502525316942,10.6996061707058,1.04548846715806));
#11337=CARTESIAN_POINT('Ctrl Pts',(10.0502525316942,10.7106795892491,1.03854944428815));
#11338=CARTESIAN_POINT('',(10.0502525316942,9.15961421508102,-0.20586304261726));
#11339=CARTESIAN_POINT('Ctrl Pts',(10.0502525316942,10.7106795892491,1.03854944428815));
#11340=CARTESIAN_POINT('Ctrl Pts',(10.0502525316942,10.7069087245865,1.00031843628634));
#11341=CARTESIAN_POINT('Ctrl Pts',(10.0502525316942,10.6988602462966,0.926048534485519));
#11342=CARTESIAN_POINT('Ctrl Pts',(10.0502525316942,10.6852672767501,0.821220046750495));
#11343=CARTESIAN_POINT('Ctrl Pts',(10.0502525316942,10.6640973524763,0.694625083433485));
#11344=CARTESIAN_POINT('Ctrl Pts',(10.0502525316942,10.6325607057952,0.55833353757036));
#11345=CARTESIAN_POINT('Ctrl Pts',(10.0502525316942,10.596013814283,0.443722777305706));
#11346=CARTESIAN_POINT('Ctrl Pts',(10.0502525316942,10.5546263356355,0.350069791437762));
#11347=CARTESIAN_POINT('Ctrl Pts',(10.0502525316942,10.5087249476599,0.275979784341797));
#11348=CARTESIAN_POINT('Ctrl Pts',(10.0502525316942,10.4588324224655,0.219218698708488));
#11349=CARTESIAN_POINT('Ctrl Pts',(10.0502525316942,10.4057430679645,0.176389733643622));
#11350=CARTESIAN_POINT('Ctrl Pts',(10.0502525316942,10.3504388022425,0.143293435954745));
#11351=CARTESIAN_POINT('Ctrl Pts',(10.0502525316942,10.2939289512549,0.115615100388502));
#11352=CARTESIAN_POINT('Ctrl Pts',(10.0502525316942,10.237110176256,0.0895255103702571));
#11353=CARTESIAN_POINT('Ctrl Pts',(10.0502525316942,10.1806284708027,0.0622734430034769));
#11354=CARTESIAN_POINT('Ctrl Pts',(10.0502525316942,10.1247109492303,0.0329060076605447));
#11355=CARTESIAN_POINT('Ctrl Pts',(10.0502525316942,10.0692584999061,0.00188374052503854));
#11356=CARTESIAN_POINT('Ctrl Pts',(10.0502525316942,10.0139888357391,-0.0295176561224909));
#11357=CARTESIAN_POINT('Ctrl Pts',(10.0502525316942,9.95855906844526,-0.0597188954606682));
#11358=CARTESIAN_POINT('Ctrl Pts',(10.0502525316942,9.90269886586131,-0.0873927181594347));
#11359=CARTESIAN_POINT('Ctrl Pts',(10.0502525316942,9.84633157004081,-0.111969973727217));
#11360=CARTESIAN_POINT('Ctrl Pts',(10.0502525316942,9.78951336137147,-0.133407037879775));
#11361=CARTESIAN_POINT('Ctrl Pts',(10.0502525316942,9.73237897573987,-0.151980202759256));
#11362=CARTESIAN_POINT('Ctrl Pts',(10.0502525316942,9.67508881816964,-0.168085081732296));
#11363=CARTESIAN_POINT('Ctrl Pts',(10.0502525316942,9.61776871087166,-0.182008602623652));
#11364=CARTESIAN_POINT('Ctrl Pts',(10.0502525316942,9.56047634174856,-0.193802962616847));
#11365=CARTESIAN_POINT('Ctrl Pts',(10.0502525316942,9.50322667013965,-0.203384169996504));
#11366=CARTESIAN_POINT('Ctrl Pts',(10.0502525316942,9.44600537601646,-0.210586047375025));
#11367=CARTESIAN_POINT('Ctrl Pts',(10.0502525316942,9.38878575682053,-0.215226755929043));
#11368=CARTESIAN_POINT('Ctrl Pts',(10.0502525316942,9.33154666905179,-0.217182662598509));
#11369=CARTESIAN_POINT('Ctrl Pts',(10.0502525316942,9.27427657522174,-0.216396922881074));
#11370=CARTESIAN_POINT('Ctrl Pts',(10.0502525316942,9.2284309476721,-0.213560366023699));
#11371=CARTESIAN_POINT('Ctrl Pts',(10.0502525316942,9.1940293375968,-0.210193044269048));
#11372=CARTESIAN_POINT('Ctrl Pts',(10.0502525316942,9.1710872092551,-0.207398059264382));
#11373=CARTESIAN_POINT('Ctrl Pts',(10.0502525316942,9.15961421508102,-0.20586304261726));
#11374=CARTESIAN_POINT('',(10.0502525316942,9.05620683581208,-1.38781479615277));
#11375=CARTESIAN_POINT('Origin',(10.0502525316942,0.,0.));
#11376=CARTESIAN_POINT('',(10.0502525316942,10.5073910450885,-2.3220627978979));
#11377=CARTESIAN_POINT('Ctrl Pts',(10.0502525316942,9.05620683581208,-1.38781479615277));
#11378=CARTESIAN_POINT('Ctrl Pts',(10.0502525316942,9.06714350898568,-1.38842685041928));
#11379=CARTESIAN_POINT('Ctrl Pts',(10.0502525316942,9.08898459591562,-1.38986102430324));
#11380=CARTESIAN_POINT('Ctrl Pts',(10.0502525316942,9.12164944850753,-1.39264248006707));
#11381=CARTESIAN_POINT('Ctrl Pts',(10.0502525316942,9.16500867538789,-1.39761376933418));
#11382=CARTESIAN_POINT('Ctrl Pts',(10.0502525316942,9.21887966989633,-1.40595054425593));
#11383=CARTESIAN_POINT('Ctrl Pts',(10.0502525316942,9.27241152635132,-1.41644161231465));
#11384=CARTESIAN_POINT('Ctrl Pts',(10.0502525316942,9.32558483941339,-1.42913234409394));
#11385=CARTESIAN_POINT('Ctrl Pts',(10.0502525316942,9.37836940755697,-1.44408281853422));
#11386=CARTESIAN_POINT('Ctrl Pts',(10.0502525316942,9.43072293720942,-1.4613660046363));
#11387=CARTESIAN_POINT('Ctrl Pts',(10.0502525316942,9.48259965202034,-1.48104540427845));
#11388=CARTESIAN_POINT('Ctrl Pts',(10.0502525316942,9.53395832441854,-1.50315324111201));
#11389=CARTESIAN_POINT('Ctrl Pts',(10.0502525316942,9.58477015487067,-1.52766939477237));
#11390=CARTESIAN_POINT('Ctrl Pts',(10.0502525316942,9.63502805143792,-1.55449526669738));
#11391=CARTESIAN_POINT('Ctrl Pts',(10.0502525316942,9.68475210162498,-1.5834404348547));
#11392=CARTESIAN_POINT('Ctrl Pts',(10.0502525316942,9.73397818528844,-1.61426576023973));
#11393=CARTESIAN_POINT('Ctrl Pts',(10.0502525316942,9.78274900943559,-1.64671853312855));
#11394=CARTESIAN_POINT('Ctrl Pts',(10.0502525316942,9.8311048104422,-1.68056831017819));
#11395=CARTESIAN_POINT('Ctrl Pts',(10.0502525316942,9.87907328228114,-1.71564646229066));
#11396=CARTESIAN_POINT('Ctrl Pts',(10.0502525316942,9.92666301240917,-1.75187093905158));
#11397=CARTESIAN_POINT('Ctrl Pts',(10.0502525316942,9.97386991924375,-1.78921666506164));
#11398=CARTESIAN_POINT('Ctrl Pts',(10.0502525316942,10.0206816495736,-1.82769447434131));
#11399=CARTESIAN_POINT('Ctrl Pts',(10.0502525316942,10.0670826197184,-1.86732763406234));
#11400=CARTESIAN_POINT('Ctrl Pts',(10.0502525316942,10.1130592286672,-1.90812724541341));
#11401=CARTESIAN_POINT('Ctrl Pts',(10.0502525316942,10.1586038807877,-1.95007408775204));
#11402=CARTESIAN_POINT('Ctrl Pts',(10.0502525316942,10.2037132140826,-1.99313042494655));
#11403=CARTESIAN_POINT('Ctrl Pts',(10.0502525316942,10.2483873017624,-2.03724707618484));
#11404=CARTESIAN_POINT('Ctrl Pts',(10.0502525316942,10.2926285935634,-2.08237185550883));
#11405=CARTESIAN_POINT('Ctrl Pts',(10.0502525316942,10.3364410841241,-2.12845748520948));
#11406=CARTESIAN_POINT('Ctrl Pts',(10.0502525316942,10.3798294947586,-2.17546854490588));
#11407=CARTESIAN_POINT('Ctrl Pts',(10.0502525316942,10.4227985654164,-2.22337966776441));
#11408=CARTESIAN_POINT('Ctrl Pts',(10.0502525316942,10.4568416324806,-2.26241558094358));
#11409=CARTESIAN_POINT('Ctrl Pts',(10.0502525316942,10.4821883711236,-2.29208631967268));
#11410=CARTESIAN_POINT('Ctrl Pts',(10.0502525316942,10.4990038742164,-2.31204152046505));
#11411=CARTESIAN_POINT('Ctrl Pts',(10.0502525316942,10.5073910450885,-2.3220627978979));
#11412=CARTESIAN_POINT('Ctrl Pts',(10.0502525316942,10.5073910450885,-2.3220627978979));
#11413=CARTESIAN_POINT('Ctrl Pts',(10.0502525316942,10.4919907084944,-2.35725738591831));
#11414=CARTESIAN_POINT('Ctrl Pts',(10.0502525316942,10.4613854889436,-2.42540514342016));
#11415=CARTESIAN_POINT('Ctrl Pts',(10.0502525316942,10.4160640224759,-2.52090250118004));
#11416=CARTESIAN_POINT('Ctrl Pts',(10.0502525316942,10.3568102329785,-2.63475959960258));
#11417=CARTESIAN_POINT('Ctrl Pts',(10.0502525316942,10.284700695789,-2.75463520264159));
#11418=CARTESIAN_POINT('Ctrl Pts',(10.0502525316942,10.214525863806,-2.85234290245999));
#11419=CARTESIAN_POINT('Ctrl Pts',(10.0502525316942,10.1462236683382,-2.92862275068379));
#11420=CARTESIAN_POINT('Ctrl Pts',(10.0502525316942,10.0796737828909,-2.98490222577489));
#11421=CARTESIAN_POINT('Ctrl Pts',(10.0502525316942,10.0146830316105,-3.02346758796109));
#11422=CARTESIAN_POINT('Ctrl Pts',(10.0502525316942,9.95095717700994,-3.04779484151101));
#11423=CARTESIAN_POINT('Ctrl Pts',(10.0502525316942,9.88813237627935,-3.06218133312374));
#11424=CARTESIAN_POINT('Ctrl Pts',(10.0502525316942,9.82583523819669,-3.07104249021943));
#11425=CARTESIAN_POINT('Ctrl Pts',(10.0502525316942,9.76373524529424,-3.07829719773955));
#11426=CARTESIAN_POINT('Ctrl Pts',(10.0502525316942,9.70159659932322,-3.08676164713489));
#11427=CARTESIAN_POINT('Ctrl Pts',(10.0502525316942,9.6393408394545,-3.09741227343545));
#11428=CARTESIAN_POINT('Ctrl Pts',(10.0502525316942,9.57701601843134,-3.10978045352405));
#11429=CARTESIAN_POINT('Ctrl Pts',(10.0502525316942,9.51474787896063,-3.12256569092544));
#11430=CARTESIAN_POINT('Ctrl Pts',(10.0502525316942,9.45269834137241,-3.13416003631015));
#11431=CARTESIAN_POINT('Ctrl Pts',(10.0502525316942,9.39102045019014,-3.14321765381094));
#11432=CARTESIAN_POINT('Ctrl Pts',(10.0502525316942,9.32981717654858,-3.14917356053584));
#11433=CARTESIAN_POINT('Ctrl Pts',(10.0502525316942,9.26915543181673,-3.1520036280196));
#11434=CARTESIAN_POINT('Ctrl Pts',(10.0502525316942,9.2090779784702,-3.15201226138312));
#11435=CARTESIAN_POINT('Ctrl Pts',(10.0502525316942,9.14961511949843,-3.14962527917495));
#11436=CARTESIAN_POINT('Ctrl Pts',(10.0502525316942,9.09079785336098,-3.14515444717397));
#11437=CARTESIAN_POINT('Ctrl Pts',(10.0502525316942,9.0326649146968,-3.13866723439399));
#11438=CARTESIAN_POINT('Ctrl Pts',(10.0502525316942,8.97525648555044,-3.13008838265685));
#11439=CARTESIAN_POINT('Ctrl Pts',(10.0502525316942,8.91861029840238,-3.11925542274306));
#11440=CARTESIAN_POINT('Ctrl Pts',(10.0502525316942,8.86275714889703,-3.10598716411038));
#11441=CARTESIAN_POINT('Ctrl Pts',(10.0502525316942,8.8077151330875,-3.09015949103058));
#11442=CARTESIAN_POINT('Ctrl Pts',(10.0502525316942,8.75349084408744,-3.07171477588927));
#11443=CARTESIAN_POINT('Ctrl Pts',(10.0502525316942,8.71076560553715,-3.0548499719756));
#11444=CARTESIAN_POINT('Ctrl Pts',(10.0502525316942,8.67908828975171,-3.04101677653125));
#11445=CARTESIAN_POINT('Ctrl Pts',(10.0502525316942,8.65813272696012,-3.0312690802849));
#11446=CARTESIAN_POINT('Ctrl Pts',(10.0502525316942,8.64769560732005,-3.02626384252387));
#11447=CARTESIAN_POINT('Origin',(29.1,0.,0.));
#11448=CARTESIAN_POINT('',(29.35,6.525,7.99082036443648E-16));
#11449=CARTESIAN_POINT('',(29.1,6.275,-7.68465866464964E-16));
#11450=CARTESIAN_POINT('Origin',(29.35,0.,0.));
#11451=CARTESIAN_POINT('Origin',(29.35,6.025,0.));
#11452=CARTESIAN_POINT('',(29.35,9.5,-1.16341445918999E-15));
#11453=CARTESIAN_POINT('Origin',(29.35,0.,0.));
#11454=CARTESIAN_POINT('Origin',(29.1,0.,0.));
#11455=CARTESIAN_POINT('',(28.85,10.,1.22464679914735E-15));
#11456=CARTESIAN_POINT('',(29.1,9.75,1.19403062916867E-15));
#11457=CARTESIAN_POINT('',(28.85,-10.,-1.22464679914735E-15));
#11458=CARTESIAN_POINT('Origin',(28.85,0.,0.));
#11459=CARTESIAN_POINT('Origin',(28.85,0.,0.));
#11460=CARTESIAN_POINT('Origin',(25.175,0.,0.));
#11461=CARTESIAN_POINT('',(25.175,-10.,-1.22464679914735E-15));
#11462=CARTESIAN_POINT('',(21.,-10.,-1.22464679914735E-15));
#11463=CARTESIAN_POINT('',(25.175,-10.,-1.22464679914735E-15));
#11464=CARTESIAN_POINT('Origin',(21.,0.,0.));
#11465=CARTESIAN_POINT('Origin',(15.75,0.,0.));
#11466=CARTESIAN_POINT('',(14.657256909085,15.1882841634002,3.83755346941362));
#11467=CARTESIAN_POINT('',(15.8,14.2806055031745,2.18414382321291));
#11468=CARTESIAN_POINT('Ctrl Pts',(14.657256909085,15.1882841634002,3.83755346941362));
#11469=CARTESIAN_POINT('Ctrl Pts',(14.6761465353606,15.2204809626378,3.62787322776073));
#11470=CARTESIAN_POINT('Ctrl Pts',(14.7000757634306,15.250028813069,3.38542345093701));
#11471=CARTESIAN_POINT('Ctrl Pts',(14.7590833374976,15.2622828979219,3.01772165354622));
#11472=CARTESIAN_POINT('Ctrl Pts',(14.7853594609317,15.2539028616426,2.91067193741133));
#11473=CARTESIAN_POINT('Ctrl Pts',(14.8353557732887,15.2268021501321,2.76471831385531));
#11474=CARTESIAN_POINT('Ctrl Pts',(14.8603859823923,15.2082738029837,2.71637224456181));
#11475=CARTESIAN_POINT('Ctrl Pts',(14.9364214749741,15.1451099616486,2.60757230132236));
#11476=CARTESIAN_POINT('Ctrl Pts',(14.9903198942808,15.0921202332377,2.57646607024933));
#11477=CARTESIAN_POINT('Ctrl Pts',(15.1263879851351,14.9660446513584,2.44988270035784));
#11478=CARTESIAN_POINT('Ctrl Pts',(15.1678275509266,14.9286624842201,2.40426863543054));
#11479=CARTESIAN_POINT('Ctrl Pts',(15.2552258947253,14.8473025034558,2.32210737310919));
#11480=CARTESIAN_POINT('Ctrl Pts',(15.3550596759664,14.7532054284997,2.23331369045724));
#11481=CARTESIAN_POINT('Ctrl Pts',(15.6054597342241,14.494507028123,2.15739979472749));
#11482=CARTESIAN_POINT('Ctrl Pts',(15.7019486088056,14.3906763868982,2.15624789525753));
#11483=CARTESIAN_POINT('Ctrl Pts',(15.8,14.2806055031745,2.18414382321291));
#11484=CARTESIAN_POINT('',(15.8,13.6345795785203,4.77539710335946));
#11485=CARTESIAN_POINT('Ctrl Pts',(15.8,13.6345795785203,4.77539710335946));
#11486=CARTESIAN_POINT('Ctrl Pts',(15.7459792937635,13.6911731184475,4.78813278866882));
#11487=CARTESIAN_POINT('Ctrl Pts',(15.6927059160363,13.7497509471747,4.79279589805565));
#11488=CARTESIAN_POINT('Ctrl Pts',(15.5867247540199,13.8716787063213,4.78623681742322));
#11489=CARTESIAN_POINT('Ctrl Pts',(15.5350561720989,13.9340337592383,4.77448531899119));
#11490=CARTESIAN_POINT('Ctrl Pts',(15.4151906303965,14.0850539296161,4.72742125274313));
#11491=CARTESIAN_POINT('Ctrl Pts',(15.3214773869192,14.2091728778631,4.67408522803015));
#11492=CARTESIAN_POINT('Ctrl Pts',(15.0123014953173,14.6493868178153,4.37489871211529));
#11493=CARTESIAN_POINT('Ctrl Pts',(14.8382414780521,14.911826741515,4.14365161073496));
#11494=CARTESIAN_POINT('Ctrl Pts',(14.657256909085,15.1882841634002,3.83755346941362));
#11495=CARTESIAN_POINT('Origin',(15.8,0.,0.));
#11496=CARTESIAN_POINT('Origin',(15.75,0.,0.));
#11497=CARTESIAN_POINT('',(14.657256909085,13.2590473860729,8.34316815560344));
#11498=CARTESIAN_POINT('',(15.8,12.9067253609027,6.49019400603778));
#11499=CARTESIAN_POINT('Ctrl Pts',(14.657256909085,13.2590473860729,8.34316815560344));
#11500=CARTESIAN_POINT('Ctrl Pts',(14.6761465353607,13.3544631198478,8.15369975356842));
#11501=CARTESIAN_POINT('Ctrl Pts',(14.7000757634309,13.4574858968645,7.93224710137492));
#11502=CARTESIAN_POINT('Ctrl Pts',(14.7590833374989,13.5827663283719,7.58632863137928));
#11503=CARTESIAN_POINT('Ctrl Pts',(14.7853594609332,13.6078766217888,7.48192872766003));
#11504=CARTESIAN_POINT('Ctrl Pts',(14.8353557732894,13.6272044635794,7.33474400248666));
#11505=CARTESIAN_POINT('Ctrl Pts',(14.8603859823931,13.6245227153103,7.2830385841017));
#11506=CARTESIAN_POINT('Ctrl Pts',(14.9364214749747,13.5980713638623,7.16004498870931));
#11507=CARTESIAN_POINT('Ctrl Pts',(14.990319894283,13.5572874913918,7.11408647834175));
#11508=CARTESIAN_POINT('Ctrl Pts',(15.1263879851328,13.4764989002042,6.95473904218075));
#11509=CARTESIAN_POINT('Ctrl Pts',(15.1678275509254,13.4550418677986,6.89980576356338));
#11510=CARTESIAN_POINT('Ctrl Pts',(15.2552258947258,13.4030531542626,6.79652414292547));
#11511=CARTESIAN_POINT('Ctrl Pts',(15.3550596759664,13.3410002748942,6.68299873715169));
#11512=CARTESIAN_POINT('Ctrl Pts',(15.6054597342243,13.1184221593503,6.53085812980638));
#11513=CARTESIAN_POINT('Ctrl Pts',(15.7019486088058,13.0200293079344,6.4976771756342));
#11514=CARTESIAN_POINT('Ctrl Pts',(15.8,12.9067253609027,6.49019400603777));
#11515=CARTESIAN_POINT('',(15.8,11.4915768952696,8.7549893339674));
#11516=CARTESIAN_POINT('Ctrl Pts',(15.8,11.4915768952696,8.7549893339674));
#11517=CARTESIAN_POINT('Ctrl Pts',(15.7459792937636,11.5414650070019,8.78459005607964));
#11518=CARTESIAN_POINT('Ctrl Pts',(15.6927059160362,11.5957348526763,8.80712648121854));
#11519=CARTESIAN_POINT('Ctrl Pts',(15.58672475402,11.7137219099126,8.83856617450447));
#11520=CARTESIAN_POINT('Ctrl Pts',(15.5350561720991,11.776656502038,8.84665860638097));
#11521=CARTESIAN_POINT('Ctrl Pts',(15.4151906304017,11.9348288154563,8.84856581863247));
#11522=CARTESIAN_POINT('Ctrl Pts',(15.321477386924,12.0693546880299,8.83619510911057));
#11523=CARTESIAN_POINT('Ctrl Pts',(15.0123014953181,12.5804767420976,8.68768541216616));
#11524=CARTESIAN_POINT('Ctrl Pts',(14.8382414780511,12.9015312258979,8.54885474594821));
#11525=CARTESIAN_POINT('Ctrl Pts',(14.657256909085,13.2590473860729,8.34316815560344));
#11526=CARTESIAN_POINT('Origin',(15.8,0.,0.));
#11527=CARTESIAN_POINT('Origin',(15.75,0.,0.));
#11528=CARTESIAN_POINT('',(14.657256909085,10.0319226693815,12.0320954124521));
#11529=CARTESIAN_POINT('',(15.8,10.2694450138623,10.160938779711));
#11530=CARTESIAN_POINT('Ctrl Pts',(14.657256909085,10.0319226693815,12.0320954124521));
#11531=CARTESIAN_POINT('Ctrl Pts',(14.6761465353608,10.1812173808714,11.8813853373316));
#11532=CARTESIAN_POINT('Ctrl Pts',(14.7000757634311,10.3476304972585,11.7026071383166));
#11533=CARTESIAN_POINT('Ctrl Pts',(14.7590833374986,10.5736739539014,11.4123329057223));
#11534=CARTESIAN_POINT('Ctrl Pts',(14.7853594609326,10.6298166065432,11.3208022043886));
#11535=CARTESIAN_POINT('Ctrl Pts',(14.8353557732898,10.6936810578157,11.1867938439891));
#11536=CARTESIAN_POINT('Ctrl Pts',(14.8603859823935,10.7071084166316,11.1367903631164));
#11537=CARTESIAN_POINT('Ctrl Pts',(14.936421474975,10.719958797647,11.0116425856352));
#11538=CARTESIAN_POINT('Ctrl Pts',(14.9903198942818,10.6953729907149,10.9553305351824));
#11539=CARTESIAN_POINT('Ctrl Pts',(15.1263879851324,10.6677795404068,10.7788170700374));
#11540=CARTESIAN_POINT('Ctrl Pts',(15.1678275509255,10.6643480065665,10.719941829784));
#11541=CARTESIAN_POINT('Ctrl Pts',(15.255225894726,10.6468195777682,10.6056497754642));
#11542=CARTESIAN_POINT('Ctrl Pts',(15.3550596759663,10.6228850621673,10.4785053042637));
#11543=CARTESIAN_POINT('Ctrl Pts',(15.6054597342236,10.4582147281995,10.2650305679762));
#11544=CARTESIAN_POINT('Ctrl Pts',(15.7019486088043,10.3748910444333,10.2030685420815));
#11545=CARTESIAN_POINT('Ctrl Pts',(15.8,10.2694450138623,10.160938779711));
#11546=CARTESIAN_POINT('',(15.8,8.22369859898568,11.8775822089691));
#11547=CARTESIAN_POINT('Ctrl Pts',(15.8,8.22369859898568,11.8775822089691));
#11548=CARTESIAN_POINT('Ctrl Pts',(15.7459792937635,8.26199788655591,11.9211504429636));
#11549=CARTESIAN_POINT('Ctrl Pts',(15.6927059160359,8.30664743856279,11.9593541615416));
#11550=CARTESIAN_POINT('Ctrl Pts',(15.58672475402,8.4091443986622,12.0257150925135));
#11551=CARTESIAN_POINT('Ctrl Pts',(15.5350561720987,8.46649805362822,12.0528593110833));
#11552=CARTESIAN_POINT('Ctrl Pts',(15.4151906304096,8.61633950199434,12.1035511106054));
#11553=CARTESIAN_POINT('Ctrl Pts',(15.3214773869304,8.74810396918937,12.1333566475148));
#11554=CARTESIAN_POINT('Ctrl Pts',(15.0123014953204,9.2801019495249,12.1500609334098));
#11555=CARTESIAN_POINT('Ctrl Pts',(14.8382414780566,9.62834394362251,12.1172364152589));
#11556=CARTESIAN_POINT('Ctrl Pts',(14.657256909085,10.0319226693815,12.0320954124521));
#11557=CARTESIAN_POINT('Origin',(15.8,0.,0.));
#11558=CARTESIAN_POINT('Origin',(15.75,0.,0.));
#11559=CARTESIAN_POINT('',(14.657256909085,5.82280346529581,14.5432373377918));
#11560=CARTESIAN_POINT('',(15.8,6.62691983743441,12.8370600702028));
#11561=CARTESIAN_POINT('Ctrl Pts',(14.657256909085,5.82280346529581,14.5432373377918));
#11562=CARTESIAN_POINT('Ctrl Pts',(14.6761465353606,6.01136314794049,14.4460381417988));
#11563=CARTESIAN_POINT('Ctrl Pts',(14.7000757634306,6.2248769283947,14.3274344517058));
#11564=CARTESIAN_POINT('Ctrl Pts',(14.7590833374957,6.52955670169151,14.121218520862));
#11565=CARTESIAN_POINT('Ctrl Pts',(14.7853594609288,6.61123607955352,14.0515166846917));
#11566=CARTESIAN_POINT('Ctrl Pts',(14.8353557732898,6.7133856428566,13.9438023610666));
#11567=CARTESIAN_POINT('Ctrl Pts',(14.8603859823939,6.74160774532212,13.9003955068086));
#11568=CARTESIAN_POINT('Ctrl Pts',(14.9364214749747,6.79250197397385,13.7853438836539));
#11569=CARTESIAN_POINT('Ctrl Pts',(14.9903198942818,6.78652086266014,13.7241905089624));
#11570=CARTESIAN_POINT('Ctrl Pts',(15.1263879851336,6.81482359240408,13.547789382642));
#11571=CARTESIAN_POINT('Ctrl Pts',(15.167827550926,6.82975345957039,13.490735299478));
#11572=CARTESIAN_POINT('Ctrl Pts',(15.2552258947248,6.84840112024766,13.3766205140753));
#11573=CARTESIAN_POINT('Ctrl Pts',(15.355059675966,6.86492784556332,13.248302764155));
#11574=CARTESIAN_POINT('Ctrl Pts',(15.6054597342238,6.7742843727849,12.9943902934785));
#11575=CARTESIAN_POINT('Ctrl Pts',(15.7019486088051,6.71418615938417,12.9097124706704));
#11576=CARTESIAN_POINT('Ctrl Pts',(15.8,6.62691983743441,12.8370600702028));
#11577=CARTESIAN_POINT('',(15.8,4.15082738595568,13.8375145813754));
#11578=CARTESIAN_POINT('Ctrl Pts',(15.8,4.15082738595568,13.8375145813754));
#11579=CARTESIAN_POINT('Ctrl Pts',(15.7459792937636,4.17378884824957,13.8907855649509));
#11580=CARTESIAN_POINT('Ctrl Pts',(15.6927059160364,4.20444749734611,13.9409169308122));
#11581=CARTESIAN_POINT('Ctrl Pts',(15.5867247540198,4.28142124371676,14.0357032291837));
#11582=CARTESIAN_POINT('Ctrl Pts',(15.5350561720987,4.32757978616832,14.0792421692081));
#11583=CARTESIAN_POINT('Ctrl Pts',(15.4151906303927,4.4544228445381,14.1737564894865));
#11584=CARTESIAN_POINT('Ctrl Pts',(15.3214773869154,4.57052788225498,14.2428206991992));
#11585=CARTESIAN_POINT('Ctrl Pts',(15.0123014953169,5.07132611986995,14.4231038360399));
#11586=CARTESIAN_POINT('Ctrl Pts',(14.8382414780529,5.41266727154756,14.4994985584882));
#11587=CARTESIAN_POINT('Ctrl Pts',(14.657256909085,5.82280346529581,14.5432373377918));
#11588=CARTESIAN_POINT('Origin',(15.8,0.,0.));
#11589=CARTESIAN_POINT('Origin',(15.75,0.,0.));
#11590=CARTESIAN_POINT('',(14.657256909085,1.04370768816965,15.6307858638156));
#11591=CARTESIAN_POINT('',(15.8,2.33570557485288,14.2566004799664));
#11592=CARTESIAN_POINT('Ctrl Pts',(14.657256909085,1.04370768816965,15.6307858638156));
#11593=CARTESIAN_POINT('Ctrl Pts',(14.6761465353608,1.25307480646283,15.5966120814786));
#11594=CARTESIAN_POINT('Ctrl Pts',(14.7000757634309,1.49278903451672,15.5497926558526));
#11595=CARTESIAN_POINT('Ctrl Pts',(14.759083337499,1.84628094545359,15.4478208788453));
#11596=CARTESIAN_POINT('Ctrl Pts',(14.7853594609334,1.94550170192429,15.4067708092064));
#11597=CARTESIAN_POINT('Ctrl Pts',(14.8353557732896,2.07593726626537,15.3358943508599));
#11598=CARTESIAN_POINT('Ctrl Pts',(14.8603859823935,2.11619153635695,15.303333088545));
#11599=CARTESIAN_POINT('Ctrl Pts',(14.9364214749743,2.20014773094338,15.2096396742024));
#11600=CARTESIAN_POINT('Ctrl Pts',(14.990319894281,2.21335678809665,15.1496310936678));
#11601=CARTESIAN_POINT('Ctrl Pts',(15.1263879851348,2.29478522950975,14.9906096774748));
#11602=CARTESIAN_POINT('Ctrl Pts',(15.1678275509262,2.32661505826123,14.9409616025797));
#11603=CARTESIAN_POINT('Ctrl Pts',(15.2552258947253,2.37961344546108,14.838194436371));
#11604=CARTESIAN_POINT('Ctrl Pts',(15.3550596759664,2.43498366067059,14.7212640431372));
#11605=CARTESIAN_POINT('Ctrl Pts',(15.605459734224,2.42723986374774,14.4517685598142));
#11606=CARTESIAN_POINT('Ctrl Pts',(15.7019486088055,2.39624995256951,14.3526637953743));
#11607=CARTESIAN_POINT('Ctrl Pts',(15.8,2.33570557485288,14.2566004799664));
#11608=CARTESIAN_POINT('',(15.8,-0.328355732126619,14.4429346149236));
#11609=CARTESIAN_POINT('Ctrl Pts',(15.8,-0.328355732126618,14.4429346149236));
#11610=CARTESIAN_POINT('Ctrl Pts',(15.7459792937636,-0.322979723020242,
14.500693813047));
#11611=CARTESIAN_POINT('Ctrl Pts',(15.6927059160364,-0.309313059018563,
14.5578456188155));
#11612=CARTESIAN_POINT('Ctrl Pts',(15.5867247540198,-0.265397252979737,
14.6717789412865));
#11613=CARTESIAN_POINT('Ctrl Pts',(15.5350561720987,-0.234952142783135,
14.7274507079624));
#11614=CARTESIAN_POINT('Ctrl Pts',(15.4151906304043,-0.143523756760452,
14.8565358287886));
#11615=CARTESIAN_POINT('Ctrl Pts',(15.321477386926,-0.0544433185749542,
14.9580982252671));
#11616=CARTESIAN_POINT('Ctrl Pts',(15.012301495319,0.366133555586479,15.2843128435225));
#11617=CARTESIAN_POINT('Ctrl Pts',(14.8382414780528,0.667161014655142,15.4624487588678));
#11618=CARTESIAN_POINT('Ctrl Pts',(14.657256909085,1.04370768816965,15.6307858638156));
#11619=CARTESIAN_POINT('Origin',(15.8,0.,0.));
#11620=CARTESIAN_POINT('Origin',(15.75,0.,0.));
#11621=CARTESIAN_POINT('',(14.657256909085,-3.83755346941362,15.1882841634002));
#11622=CARTESIAN_POINT('',(15.8,-2.18414382321291,14.2806055031745));
#11623=CARTESIAN_POINT('Ctrl Pts',(14.657256909085,-3.83755346941362,15.1882841634002));
#11624=CARTESIAN_POINT('Ctrl Pts',(14.6761465353606,-3.62787322776029,15.2204809626379));
#11625=CARTESIAN_POINT('Ctrl Pts',(14.7000757634306,-3.38542345093672,15.2500288130691));
#11626=CARTESIAN_POINT('Ctrl Pts',(14.7590833374979,-3.01772165354433,15.2622828979219));
#11627=CARTESIAN_POINT('Ctrl Pts',(14.7853594609321,-2.91067193741018,15.2539028616423));
#11628=CARTESIAN_POINT('Ctrl Pts',(14.8353557732891,-2.76471831385429,15.226802150132));
#11629=CARTESIAN_POINT('Ctrl Pts',(14.8603859823928,-2.71637224456103,15.2082738029833));
#11630=CARTESIAN_POINT('Ctrl Pts',(14.9364214749744,-2.60757230132201,15.1451099616484));
#11631=CARTESIAN_POINT('Ctrl Pts',(14.9903198942815,-2.57646607024861,15.092120233237));
#11632=CARTESIAN_POINT('Ctrl Pts',(15.1263879851344,-2.44988270035848,14.9660446513591));
#11633=CARTESIAN_POINT('Ctrl Pts',(15.1678275509266,-2.4042686354305,14.9286624842201));
#11634=CARTESIAN_POINT('Ctrl Pts',(15.2552258947252,-2.32210737310926,14.8473025034559));
#11635=CARTESIAN_POINT('Ctrl Pts',(15.3550596759664,-2.23331369045724,14.7532054284997));
#11636=CARTESIAN_POINT('Ctrl Pts',(15.605459734224,-2.1573997947275,14.4945070281231));
#11637=CARTESIAN_POINT('Ctrl Pts',(15.7019486088056,-2.15624789525753,14.3906763868982));
#11638=CARTESIAN_POINT('Ctrl Pts',(15.8,-2.18414382321291,14.2806055031745));
#11639=CARTESIAN_POINT('',(15.8,-4.77539710335946,13.6345795785203));
#11640=CARTESIAN_POINT('Ctrl Pts',(15.8,-4.77539710335946,13.6345795785203));
#11641=CARTESIAN_POINT('Ctrl Pts',(15.7459792937632,-4.78813278866891,13.6911731184479));
#11642=CARTESIAN_POINT('Ctrl Pts',(15.692705916036,-4.79279589805564,13.749750947175));
#11643=CARTESIAN_POINT('Ctrl Pts',(15.5867247540198,-4.78623681742321,13.8716787063214));
#11644=CARTESIAN_POINT('Ctrl Pts',(15.5350561720987,-4.77448531899113,13.9340337592385));
#11645=CARTESIAN_POINT('Ctrl Pts',(15.4151906304068,-4.72742125274714,14.0850539296032));
#11646=CARTESIAN_POINT('Ctrl Pts',(15.3214773869283,-4.67408522803895,14.2091728778501));
#11647=CARTESIAN_POINT('Ctrl Pts',(15.0123014953194,-4.37489871211733,14.6493868178123));
#11648=CARTESIAN_POINT('Ctrl Pts',(14.8382414780541,-4.14365161073839,14.9118267415119));
#11649=CARTESIAN_POINT('Ctrl Pts',(14.657256909085,-3.83755346941362,15.1882841634002));
#11650=CARTESIAN_POINT('Origin',(15.8,0.,0.));
#11651=CARTESIAN_POINT('Origin',(15.75,0.,0.));
#11652=CARTESIAN_POINT('',(14.657256909085,-8.34316815560344,13.2590473860729));
#11653=CARTESIAN_POINT('',(15.8,-6.49019400603777,12.9067253609027));
#11654=CARTESIAN_POINT('Ctrl Pts',(14.657256909085,-8.34316815560344,13.2590473860729));
#11655=CARTESIAN_POINT('Ctrl Pts',(14.6761465353607,-8.15369975356933,13.3544631198474));
#11656=CARTESIAN_POINT('Ctrl Pts',(14.7000757634308,-7.93224710137545,13.4574858968644));
#11657=CARTESIAN_POINT('Ctrl Pts',(14.7590833374967,-7.58632863139194,13.5827663283673));
#11658=CARTESIAN_POINT('Ctrl Pts',(14.7853594609301,-7.48192872766908,13.6078766217876));
#11659=CARTESIAN_POINT('Ctrl Pts',(14.8353557732899,-7.33474400248519,13.6272044635796));
#11660=CARTESIAN_POINT('Ctrl Pts',(14.8603859823939,-7.28303858410022,13.62452271531));
#11661=CARTESIAN_POINT('Ctrl Pts',(14.9364214749749,-7.16004498870914,13.5980713638622));
#11662=CARTESIAN_POINT('Ctrl Pts',(14.9903198942826,-7.11408647834217,13.5572874913921));
#11663=CARTESIAN_POINT('Ctrl Pts',(15.1263879851326,-6.95473904218106,13.4764989002043));
#11664=CARTESIAN_POINT('Ctrl Pts',(15.1678275509258,-6.89980576356297,13.4550418677983));
#11665=CARTESIAN_POINT('Ctrl Pts',(15.2552258947243,-6.79652414292717,13.4030531542635));
#11666=CARTESIAN_POINT('Ctrl Pts',(15.3550596759657,-6.6829987371522,13.3410002748947));
#11667=CARTESIAN_POINT('Ctrl Pts',(15.6054597342234,-6.53085812980684,13.1184221593511));
#11668=CARTESIAN_POINT('Ctrl Pts',(15.7019486088045,-6.49767717563431,13.0200293079359));
#11669=CARTESIAN_POINT('Ctrl Pts',(15.8,-6.49019400603777,12.9067253609027));
#11670=CARTESIAN_POINT('',(15.8,-8.7549893339674,11.4915768952696));
#11671=CARTESIAN_POINT('Ctrl Pts',(15.8,-8.7549893339674,11.4915768952696));
#11672=CARTESIAN_POINT('Ctrl Pts',(15.7459792937626,-8.78459005608021,11.5414650070028));
#11673=CARTESIAN_POINT('Ctrl Pts',(15.6927059160353,-8.80712648121881,11.5957348526773));
#11674=CARTESIAN_POINT('Ctrl Pts',(15.5867247540199,-8.83856617450449,11.7137219099127));
#11675=CARTESIAN_POINT('Ctrl Pts',(15.5350561720989,-8.84665860638097,11.7766565020382));
#11676=CARTESIAN_POINT('Ctrl Pts',(15.4151906303964,-8.84856581863256,11.9348288154633));
#11677=CARTESIAN_POINT('Ctrl Pts',(15.3214773869192,-8.83619510910824,12.0693546880378));
#11678=CARTESIAN_POINT('Ctrl Pts',(15.0123014953169,-8.68768541216563,12.5804767420995));
#11679=CARTESIAN_POINT('Ctrl Pts',(14.8382414780509,-8.54885474594795,12.9015312258984));
#11680=CARTESIAN_POINT('Ctrl Pts',(14.657256909085,-8.34316815560344,13.2590473860729));
#11681=CARTESIAN_POINT('Origin',(15.8,0.,0.));
#11682=CARTESIAN_POINT('Origin',(15.75,0.,0.));
#11683=CARTESIAN_POINT('',(14.657256909085,-12.0320954124521,10.0319226693815));
#11684=CARTESIAN_POINT('',(15.8,-10.160938779711,10.2694450138623));
#11685=CARTESIAN_POINT('Ctrl Pts',(14.657256909085,-12.0320954124521,10.0319226693815));
#11686=CARTESIAN_POINT('Ctrl Pts',(14.6761465353606,-11.8813853373331,10.1812173808699));
#11687=CARTESIAN_POINT('Ctrl Pts',(14.7000757634307,-11.7026071383195,10.3476304972558));
#11688=CARTESIAN_POINT('Ctrl Pts',(14.7590833374962,-11.4123329057338,10.5736739538928));
#11689=CARTESIAN_POINT('Ctrl Pts',(14.7853594609295,-11.3208022043972,10.6298166065389));
#11690=CARTESIAN_POINT('Ctrl Pts',(14.8353557732893,-11.1867938439903,10.6936810578153));
#11691=CARTESIAN_POINT('Ctrl Pts',(14.860385982393,-11.1367903631174,10.7071084166315));
#11692=CARTESIAN_POINT('Ctrl Pts',(14.9364214749746,-11.0116425856357,10.7199587976471));
#11693=CARTESIAN_POINT('Ctrl Pts',(14.9903198942805,-10.9553305351842,10.6953729907151));
#11694=CARTESIAN_POINT('Ctrl Pts',(15.1263879851341,-10.7788170700351,10.6677795404065));
#11695=CARTESIAN_POINT('Ctrl Pts',(15.1678275509254,-10.719941829784,10.6643480065666));
#11696=CARTESIAN_POINT('Ctrl Pts',(15.2552258947242,-10.6056497754665,10.6468195777685));
#11697=CARTESIAN_POINT('Ctrl Pts',(15.3550596759655,-10.4785053042644,10.6228850621678));
#11698=CARTESIAN_POINT('Ctrl Pts',(15.605459734223,-10.2650305679767,10.4582147281999));
#11699=CARTESIAN_POINT('Ctrl Pts',(15.7019486088037,-10.2030685420817,10.3748910444339));
#11700=CARTESIAN_POINT('Ctrl Pts',(15.8,-10.160938779711,10.2694450138623));
#11701=CARTESIAN_POINT('',(15.8,-11.8775822089691,8.22369859898568));
#11702=CARTESIAN_POINT('Ctrl Pts',(15.8,-11.8775822089691,8.22369859898568));
#11703=CARTESIAN_POINT('Ctrl Pts',(15.7459792937652,-11.9211504429623,8.26199788655478));
#11704=CARTESIAN_POINT('Ctrl Pts',(15.6927059160382,-11.9593541615401,8.30664743856047));
#11705=CARTESIAN_POINT('Ctrl Pts',(15.5867247540197,-12.0257150925138,8.40914439866259));
#11706=CARTESIAN_POINT('Ctrl Pts',(15.5350561720987,-12.0528593110834,8.4664980536283));
#11707=CARTESIAN_POINT('Ctrl Pts',(15.4151906304064,-12.1035511106068,8.61633950199834));
#11708=CARTESIAN_POINT('Ctrl Pts',(15.321477386928,-12.1333566475149,8.74810396919347));
#11709=CARTESIAN_POINT('Ctrl Pts',(15.0123014953193,-12.1500609334098,9.28010194952675));
#11710=CARTESIAN_POINT('Ctrl Pts',(14.8382414780578,-12.1172364152594,9.62834394361986));
#11711=CARTESIAN_POINT('Ctrl Pts',(14.657256909085,-12.0320954124521,10.0319226693815));
#11712=CARTESIAN_POINT('Origin',(15.8,0.,0.));
#11713=CARTESIAN_POINT('Origin',(15.75,0.,0.));
#11714=CARTESIAN_POINT('',(14.657256909085,-14.5432373377918,5.82280346529581));
#11715=CARTESIAN_POINT('',(15.8,-12.8370600702028,6.62691983743441));
#11716=CARTESIAN_POINT('Ctrl Pts',(14.657256909085,-14.5432373377918,5.82280346529581));
#11717=CARTESIAN_POINT('Ctrl Pts',(14.6761465353606,-14.4460381417986,6.01136314794083));
#11718=CARTESIAN_POINT('Ctrl Pts',(14.7000757634306,-14.327434451706,6.22487692839421));
#11719=CARTESIAN_POINT('Ctrl Pts',(14.7590833374988,-14.1212185208509,6.52955670170803));
#11720=CARTESIAN_POINT('Ctrl Pts',(14.7853594609333,-14.0515166846818,6.61123607956297));
#11721=CARTESIAN_POINT('Ctrl Pts',(14.8353557732886,-13.9438023610692,6.71338564285407));
#11722=CARTESIAN_POINT('Ctrl Pts',(14.860385982392,-13.9003955068115,6.74160774532081));
#11723=CARTESIAN_POINT('Ctrl Pts',(14.9364214749746,-13.7853438836541,6.79250197397384));
#11724=CARTESIAN_POINT('Ctrl Pts',(14.9903198942818,-13.7241905089624,6.78652086266011));
#11725=CARTESIAN_POINT('Ctrl Pts',(15.1263879851336,-13.5477893826419,6.81482359240412));
#11726=CARTESIAN_POINT('Ctrl Pts',(15.167827550926,-13.490735299478,6.82975345957041));
#11727=CARTESIAN_POINT('Ctrl Pts',(15.2552258947255,-13.3766205140743,6.84840112024782));
#11728=CARTESIAN_POINT('Ctrl Pts',(15.3550596759663,-13.2483027641547,6.86492784556322));
#11729=CARTESIAN_POINT('Ctrl Pts',(15.6054597342241,-12.9943902934783,6.7742843727848));
#11730=CARTESIAN_POINT('Ctrl Pts',(15.7019486088055,-12.9097124706701,6.71418615938381));
#11731=CARTESIAN_POINT('Ctrl Pts',(15.8,-12.8370600702028,6.62691983743441));
#11732=CARTESIAN_POINT('',(15.8,-13.8375145813754,4.15082738595568));
#11733=CARTESIAN_POINT('Ctrl Pts',(15.8,-13.8375145813754,4.15082738595568));
#11734=CARTESIAN_POINT('Ctrl Pts',(15.7459792937635,-13.8907855649511,4.17378884824963));
#11735=CARTESIAN_POINT('Ctrl Pts',(15.6927059160365,-13.9409169308122,4.20444749734604));
#11736=CARTESIAN_POINT('Ctrl Pts',(15.5867247540197,-14.0357032291838,4.28142124371689));
#11737=CARTESIAN_POINT('Ctrl Pts',(15.5350561720985,-14.0792421692082,4.3275797861685));
#11738=CARTESIAN_POINT('Ctrl Pts',(15.4151906303655,-14.1737564895079,4.45442284456682));
#11739=CARTESIAN_POINT('Ctrl Pts',(15.3214773868911,-14.2428206992134,4.57052788229435));
#11740=CARTESIAN_POINT('Ctrl Pts',(15.0123014953115,-14.423103836043,5.07132611987859));
#11741=CARTESIAN_POINT('Ctrl Pts',(14.8382414780483,-14.4994985584893,5.41266727155799));
#11742=CARTESIAN_POINT('Ctrl Pts',(14.657256909085,-14.5432373377918,5.82280346529581));
#11743=CARTESIAN_POINT('Origin',(15.8,0.,0.));
#11744=CARTESIAN_POINT('Origin',(15.75,0.,0.));
#11745=CARTESIAN_POINT('',(14.657256909085,-15.6307858638156,1.04370768816965));
#11746=CARTESIAN_POINT('',(15.8,-14.2566004799664,2.33570557485288));
#11747=CARTESIAN_POINT('Ctrl Pts',(14.657256909085,-15.6307858638156,1.04370768816965));
#11748=CARTESIAN_POINT('Ctrl Pts',(14.6761465353606,-15.5966120814789,1.25307480646121));
#11749=CARTESIAN_POINT('Ctrl Pts',(14.7000757634306,-15.549792655853,1.49278903451451));
#11750=CARTESIAN_POINT('Ctrl Pts',(14.7590833374982,-15.4478208788467,1.84628094544931));
#11751=CARTESIAN_POINT('Ctrl Pts',(14.7853594609325,-15.4067708092076,1.94550170192191));
#11752=CARTESIAN_POINT('Ctrl Pts',(14.8353557732886,-15.3358943508614,2.07593726626272));
#11753=CARTESIAN_POINT('Ctrl Pts',(14.860385982392,-15.3033330885469,2.11619153635516));
#11754=CARTESIAN_POINT('Ctrl Pts',(14.9364214749742,-15.2096396742025,2.2001477309434));
#11755=CARTESIAN_POINT('Ctrl Pts',(14.9903198942811,-15.1496310936678,2.2133567880966));
#11756=CARTESIAN_POINT('Ctrl Pts',(15.126387985135,-14.9906096774745,2.29478522950994));
#11757=CARTESIAN_POINT('Ctrl Pts',(15.1678275509263,-14.9409616025796,2.32661505826135));
#11758=CARTESIAN_POINT('Ctrl Pts',(15.2552258947247,-14.8381944363718,2.37961344546068));
#11759=CARTESIAN_POINT('Ctrl Pts',(15.3550596759661,-14.7212640431375,2.43498366067061));
#11760=CARTESIAN_POINT('Ctrl Pts',(15.6054597342239,-14.4517685598143,2.42723986374774));
#11761=CARTESIAN_POINT('Ctrl Pts',(15.7019486088054,-14.3526637953743,2.39624995256956));
#11762=CARTESIAN_POINT('Ctrl Pts',(15.8,-14.2566004799664,2.33570557485288));
#11763=CARTESIAN_POINT('',(15.8,-14.4429346149236,-0.328355732126617));
#11764=CARTESIAN_POINT('Ctrl Pts',(15.8,-14.4429346149236,-0.328355732126619));
#11765=CARTESIAN_POINT('Ctrl Pts',(15.7459792937635,-14.5006938130472,-0.322979723020233));
#11766=CARTESIAN_POINT('Ctrl Pts',(15.6927059160363,-14.5578456188156,-0.309313059018514));
#11767=CARTESIAN_POINT('Ctrl Pts',(15.5867247540198,-14.6717789412865,-0.265397252979746));
#11768=CARTESIAN_POINT('Ctrl Pts',(15.5350561720988,-14.7274507079622,-0.234952142783211));
#11769=CARTESIAN_POINT('Ctrl Pts',(15.4151906304082,-14.8565358287844,-0.143523756763411));
#11770=CARTESIAN_POINT('Ctrl Pts',(15.3214773869296,-14.9580982252633,-0.05444331857987));
#11771=CARTESIAN_POINT('Ctrl Pts',(15.0123014953195,-15.2843128435219,0.366133555585719));
#11772=CARTESIAN_POINT('Ctrl Pts',(14.8382414780523,-15.4624487588682,0.667161014656064));
#11773=CARTESIAN_POINT('Ctrl Pts',(14.657256909085,-15.6307858638156,1.04370768816965));
#11774=CARTESIAN_POINT('Origin',(15.8,0.,0.));
#11775=CARTESIAN_POINT('Origin',(15.75,0.,0.));
#11776=CARTESIAN_POINT('',(14.657256909085,-15.1882841634002,-3.83755346941362));
#11777=CARTESIAN_POINT('',(15.8,-14.2806055031745,-2.18414382321291));
#11778=CARTESIAN_POINT('Ctrl Pts',(14.657256909085,-15.1882841634002,-3.83755346941362));
#11779=CARTESIAN_POINT('Ctrl Pts',(14.6761465353606,-15.2204809626379,-3.62787322776027));
#11780=CARTESIAN_POINT('Ctrl Pts',(14.7000757634307,-15.2500288130692,-3.38542345093602));
#11781=CARTESIAN_POINT('Ctrl Pts',(14.7590833374981,-15.2622828979219,-3.01772165354352));
#11782=CARTESIAN_POINT('Ctrl Pts',(14.7853594609323,-15.2539028616423,-2.91067193740946));
#11783=CARTESIAN_POINT('Ctrl Pts',(14.8353557732889,-15.226802150132,-2.76471831385505));
#11784=CARTESIAN_POINT('Ctrl Pts',(14.8603859823924,-15.2082738029837,-2.7163722445616));
#11785=CARTESIAN_POINT('Ctrl Pts',(14.9364214749744,-15.1451099616484,-2.60757230132212));
#11786=CARTESIAN_POINT('Ctrl Pts',(14.9903198942815,-15.092120233237,-2.5764660702486));
#11787=CARTESIAN_POINT('Ctrl Pts',(15.1263879851341,-14.9660446513593,-2.44988270035873));
#11788=CARTESIAN_POINT('Ctrl Pts',(15.1678275509262,-14.9286624842204,-2.40426863543085));
#11789=CARTESIAN_POINT('Ctrl Pts',(15.2552258947263,-14.8473025034548,-2.32210737310816));
#11790=CARTESIAN_POINT('Ctrl Pts',(15.3550596759668,-14.7532054284993,-2.23331369045709));
#11791=CARTESIAN_POINT('Ctrl Pts',(15.6054597342245,-14.4945070281226,-2.15739979472738));
#11792=CARTESIAN_POINT('Ctrl Pts',(15.7019486088061,-14.3906763868977,-2.15624789525766));
#11793=CARTESIAN_POINT('Ctrl Pts',(15.8,-14.2806055031745,-2.18414382321291));
#11794=CARTESIAN_POINT('',(15.8,-13.6345795785203,-4.77539710335946));
#11795=CARTESIAN_POINT('Ctrl Pts',(15.8,-13.6345795785203,-4.77539710335946));
#11796=CARTESIAN_POINT('Ctrl Pts',(15.7459792937634,-13.6911731184477,-4.78813278866886));
#11797=CARTESIAN_POINT('Ctrl Pts',(15.6927059160361,-13.7497509471749,-4.79279589805564));
#11798=CARTESIAN_POINT('Ctrl Pts',(15.5867247540198,-13.8716787063213,-4.78623681742322));
#11799=CARTESIAN_POINT('Ctrl Pts',(15.5350561720989,-13.9340337592383,-4.77448531899119));
#11800=CARTESIAN_POINT('Ctrl Pts',(15.4151906304075,-14.0850539296022,-4.72742125274744));
#11801=CARTESIAN_POINT('Ctrl Pts',(15.3214773869291,-14.2091728778489,-4.67408522803976));
#11802=CARTESIAN_POINT('Ctrl Pts',(15.0123014953194,-14.6493868178123,-4.3748987121173));
#11803=CARTESIAN_POINT('Ctrl Pts',(14.8382414780541,-14.911826741512,-4.14365161073832));
#11804=CARTESIAN_POINT('Ctrl Pts',(14.657256909085,-15.1882841634002,-3.83755346941362));
#11805=CARTESIAN_POINT('Origin',(15.8,0.,0.));
#11806=CARTESIAN_POINT('Origin',(15.75,0.,0.));
#11807=CARTESIAN_POINT('',(14.657256909085,-13.2590473860729,-8.34316815560344));
#11808=CARTESIAN_POINT('',(15.8,-12.9067253609027,-6.49019400603777));
#11809=CARTESIAN_POINT('Ctrl Pts',(14.657256909085,-13.2590473860729,-8.34316815560344));
#11810=CARTESIAN_POINT('Ctrl Pts',(14.6761465353605,-13.3544631198464,-8.15369975357118));
#11811=CARTESIAN_POINT('Ctrl Pts',(14.7000757634303,-13.4574858968621,-7.93224710138034));
#11812=CARTESIAN_POINT('Ctrl Pts',(14.7590833374966,-13.582766328368,-7.58632863139116));
#11813=CARTESIAN_POINT('Ctrl Pts',(14.7853594609306,-13.6078766217876,-7.48192872766814));
#11814=CARTESIAN_POINT('Ctrl Pts',(14.8353557732881,-13.6272044635792,-7.33474400249002));
#11815=CARTESIAN_POINT('Ctrl Pts',(14.8603859823915,-13.6245227153108,-7.28303858410438));
#11816=CARTESIAN_POINT('Ctrl Pts',(14.936421474974,-13.5980713638627,-7.16004498871016));
#11817=CARTESIAN_POINT('Ctrl Pts',(14.9903198942806,-13.5572874913932,-7.11408647834473));
#11818=CARTESIAN_POINT('Ctrl Pts',(15.1263879851354,-13.4764989002027,-6.95473904217766));
#11819=CARTESIAN_POINT('Ctrl Pts',(15.1678275509263,-13.455041867798,-6.89980576356226));
#11820=CARTESIAN_POINT('Ctrl Pts',(15.2552258947274,-13.4030531542616,-6.7965241429236));
#11821=CARTESIAN_POINT('Ctrl Pts',(15.3550596759675,-13.3410002748933,-6.68299873715091));
#11822=CARTESIAN_POINT('Ctrl Pts',(15.6054597342251,-13.1184221593495,-6.53085812980596));
#11823=CARTESIAN_POINT('Ctrl Pts',(15.7019486088073,-13.0200293079327,-6.49767717563406));
#11824=CARTESIAN_POINT('Ctrl Pts',(15.8,-12.9067253609027,-6.49019400603777));
#11825=CARTESIAN_POINT('',(15.8,-11.4915768952696,-8.7549893339674));
#11826=CARTESIAN_POINT('Ctrl Pts',(15.8,-11.4915768952696,-8.7549893339674));
#11827=CARTESIAN_POINT('Ctrl Pts',(15.7459792937642,-11.5414650070013,-8.78459005607929));
#11828=CARTESIAN_POINT('Ctrl Pts',(15.6927059160377,-11.5957348526747,-8.80712648121812));
#11829=CARTESIAN_POINT('Ctrl Pts',(15.5867247540194,-11.7137219099132,-8.83856617450462));
#11830=CARTESIAN_POINT('Ctrl Pts',(15.5350561720984,-11.7766565020389,-8.84665860638099));
#11831=CARTESIAN_POINT('Ctrl Pts',(15.4151906304178,-11.934828815435,-8.8485658186322));
#11832=CARTESIAN_POINT('Ctrl Pts',(15.321477386938,-12.0693546880067,-8.83619510911733));
#11833=CARTESIAN_POINT('Ctrl Pts',(15.0123014953219,-12.5804767420913,-8.68768541216795));
#11834=CARTESIAN_POINT('Ctrl Pts',(14.8382414780576,-12.9015312258851,-8.54885474595556));
#11835=CARTESIAN_POINT('Ctrl Pts',(14.657256909085,-13.2590473860729,-8.34316815560344));
#11836=CARTESIAN_POINT('Origin',(15.8,0.,0.));
#11837=CARTESIAN_POINT('Origin',(15.75,0.,0.));
#11838=CARTESIAN_POINT('',(14.657256909085,-10.0319226693815,-12.0320954124521));
#11839=CARTESIAN_POINT('',(15.8,-10.2694450138623,-10.160938779711));
#11840=CARTESIAN_POINT('Ctrl Pts',(14.657256909085,-10.0319226693815,-12.0320954124521));
#11841=CARTESIAN_POINT('Ctrl Pts',(14.6761465353604,-10.1812173808683,-11.8813853373348));
#11842=CARTESIAN_POINT('Ctrl Pts',(14.7000757634301,-10.3476304972515,-11.7026071383242));
#11843=CARTESIAN_POINT('Ctrl Pts',(14.7590833374954,-10.5736739538916,-11.412332905736));
#11844=CARTESIAN_POINT('Ctrl Pts',(14.7853594609291,-10.6298166065378,-11.3208022043988));
#11845=CARTESIAN_POINT('Ctrl Pts',(14.8353557732878,-10.693681057814,-11.1867938439937));
#11846=CARTESIAN_POINT('Ctrl Pts',(14.8603859823911,-10.7071084166306,-11.1367903631209));
#11847=CARTESIAN_POINT('Ctrl Pts',(14.9364214749739,-10.7199587976481,-11.0116425856358));
#11848=CARTESIAN_POINT('Ctrl Pts',(14.9903198942828,-10.695372990714,-10.9553305351818));
#11849=CARTESIAN_POINT('Ctrl Pts',(15.126387985135,-10.6677795404067,-10.7788170700337));
#11850=CARTESIAN_POINT('Ctrl Pts',(15.1678275509272,-10.6643480065664,-10.7199418297816));
#11851=CARTESIAN_POINT('Ctrl Pts',(15.2552258947223,-10.6468195777688,-10.6056497754691));
#11852=CARTESIAN_POINT('Ctrl Pts',(15.3550596759653,-10.6228850621681,-10.4785053042643));
#11853=CARTESIAN_POINT('Ctrl Pts',(15.6054597342239,-10.4582147281991,-10.2650305679761));
#11854=CARTESIAN_POINT('Ctrl Pts',(15.701948608806,-10.3748910444315,-10.2030685420807));
#11855=CARTESIAN_POINT('Ctrl Pts',(15.8,-10.2694450138623,-10.160938779711));
#11856=CARTESIAN_POINT('',(15.8,-8.22369859898568,-11.8775822089691));
#11857=CARTESIAN_POINT('Ctrl Pts',(15.8,-8.22369859898568,-11.8775822089691));
#11858=CARTESIAN_POINT('Ctrl Pts',(15.7459792937643,-8.26199788655536,-11.9211504429629));
#11859=CARTESIAN_POINT('Ctrl Pts',(15.6927059160378,-8.30664743856085,-11.9593541615403));
#11860=CARTESIAN_POINT('Ctrl Pts',(15.5867247540195,-8.40914439866277,-12.0257150925139));
#11861=CARTESIAN_POINT('Ctrl Pts',(15.5350561720988,-8.46649805362819,-12.0528593110833));
#11862=CARTESIAN_POINT('Ctrl Pts',(15.4151906304098,-8.616339501994,-12.1035511106053));
#11863=CARTESIAN_POINT('Ctrl Pts',(15.3214773869315,-8.74810396918746,-12.1333566475148));
#11864=CARTESIAN_POINT('Ctrl Pts',(15.0123014953196,-9.28010194952635,-12.1500609334098));
#11865=CARTESIAN_POINT('Ctrl Pts',(14.838241478058,-9.62834394361936,-12.1172364152595));
#11866=CARTESIAN_POINT('Ctrl Pts',(14.657256909085,-10.0319226693815,-12.0320954124521));
#11867=CARTESIAN_POINT('Origin',(15.8,0.,0.));
#11868=CARTESIAN_POINT('Origin',(15.75,0.,0.));
#11869=CARTESIAN_POINT('',(14.657256909085,-5.82280346529581,-14.5432373377918));
#11870=CARTESIAN_POINT('',(15.8,-6.62691983743441,-12.8370600702028));
#11871=CARTESIAN_POINT('Ctrl Pts',(14.657256909085,-5.82280346529581,-14.5432373377918));
#11872=CARTESIAN_POINT('Ctrl Pts',(14.6761465353607,-6.01136314794179,-14.4460381417981));
#11873=CARTESIAN_POINT('Ctrl Pts',(14.700075763431,-6.22487692839756,-14.3274344517042));
#11874=CARTESIAN_POINT('Ctrl Pts',(14.7590833374979,-6.52955670170211,-14.1212185208546));
#11875=CARTESIAN_POINT('Ctrl Pts',(14.7853594609316,-6.61123607955977,-14.0515166846853));
#11876=CARTESIAN_POINT('Ctrl Pts',(14.8353557732899,-6.71338564285629,-13.9438023610667));
#11877=CARTESIAN_POINT('Ctrl Pts',(14.8603859823937,-6.74160774532217,-13.9003955068088));
#11878=CARTESIAN_POINT('Ctrl Pts',(14.9364214749747,-6.79250197397347,-13.7853438836541));
#11879=CARTESIAN_POINT('Ctrl Pts',(14.9903198942808,-6.78652086266014,-13.7241905089635));
#11880=CARTESIAN_POINT('Ctrl Pts',(15.1263879851336,-6.81482359240397,-13.547789382642));
#11881=CARTESIAN_POINT('Ctrl Pts',(15.1678275509249,-6.82975345957013,-13.4907352994794));
#11882=CARTESIAN_POINT('Ctrl Pts',(15.2552258947256,-6.84840112024788,-13.3766205140742));
#11883=CARTESIAN_POINT('Ctrl Pts',(15.3550596759661,-6.8649278455632,-13.248302764155));
#11884=CARTESIAN_POINT('Ctrl Pts',(15.6054597342236,-6.77428437278503,-12.9943902934787));
#11885=CARTESIAN_POINT('Ctrl Pts',(15.7019486088046,-6.71418615938468,-12.9097124706708));
#11886=CARTESIAN_POINT('Ctrl Pts',(15.8,-6.62691983743441,-12.8370600702028));
#11887=CARTESIAN_POINT('',(15.8,-4.15082738595568,-13.8375145813754));
#11888=CARTESIAN_POINT('Ctrl Pts',(15.8,-4.15082738595568,-13.8375145813754));
#11889=CARTESIAN_POINT('Ctrl Pts',(15.7459792937636,-4.17378884824959,-13.890785564951));
#11890=CARTESIAN_POINT('Ctrl Pts',(15.6927059160362,-4.20444749734624,-13.9409169308124));
#11891=CARTESIAN_POINT('Ctrl Pts',(15.5867247540199,-4.28142124371671,-14.0357032291836));
#11892=CARTESIAN_POINT('Ctrl Pts',(15.5350561720989,-4.32757978616817,-14.079242169208));
#11893=CARTESIAN_POINT('Ctrl Pts',(15.415190630367,-4.45442284456523,-14.1737564895067));
#11894=CARTESIAN_POINT('Ctrl Pts',(15.3214773868927,-4.57052788229179,-14.2428206992125));
#11895=CARTESIAN_POINT('Ctrl Pts',(15.0123014953115,-5.07132611987859,-14.423103836043));
#11896=CARTESIAN_POINT('Ctrl Pts',(14.8382414780483,-5.41266727155799,-14.4994985584893));
#11897=CARTESIAN_POINT('Ctrl Pts',(14.657256909085,-5.82280346529581,-14.5432373377918));
#11898=CARTESIAN_POINT('Origin',(15.8,0.,0.));
#11899=CARTESIAN_POINT('Origin',(15.75,0.,0.));
#11900=CARTESIAN_POINT('',(14.657256909085,-1.04370768816965,-15.6307858638156));
#11901=CARTESIAN_POINT('',(15.8,-2.33570557485288,-14.2566004799664));
#11902=CARTESIAN_POINT('Ctrl Pts',(14.657256909085,-1.04370768816965,-15.6307858638156));
#11903=CARTESIAN_POINT('Ctrl Pts',(14.6761465353607,-1.25307480646202,-15.5966120814788));
#11904=CARTESIAN_POINT('Ctrl Pts',(14.7000757634309,-1.49278903451753,-15.5497926558525));
#11905=CARTESIAN_POINT('Ctrl Pts',(14.7590833374979,-1.84628094544666,-15.4478208788472));
#11906=CARTESIAN_POINT('Ctrl Pts',(14.7853594609317,-1.94550170192027,-15.4067708092087));
#11907=CARTESIAN_POINT('Ctrl Pts',(14.8353557732893,-2.07593726626439,-15.3358943508604));
#11908=CARTESIAN_POINT('Ctrl Pts',(14.8603859823929,-2.11619153635627,-15.3033330885458));
#11909=CARTESIAN_POINT('Ctrl Pts',(14.9364214749743,-2.20014773094341,-15.2096396742024));
#11910=CARTESIAN_POINT('Ctrl Pts',(14.9903198942815,-2.21335678809698,-15.1496310936672));
#11911=CARTESIAN_POINT('Ctrl Pts',(15.1263879851342,-2.29478522950942,-14.9906096774754));
#11912=CARTESIAN_POINT('Ctrl Pts',(15.1678275509262,-2.32661505826123,-14.9409616025797));
#11913=CARTESIAN_POINT('Ctrl Pts',(15.2552258947253,-2.37961344546106,-14.8381944363711));
#11914=CARTESIAN_POINT('Ctrl Pts',(15.3550596759663,-2.43498366067057,-14.7212640431373));
#11915=CARTESIAN_POINT('Ctrl Pts',(15.605459734224,-2.42723986374776,-14.4517685598143));
#11916=CARTESIAN_POINT('Ctrl Pts',(15.7019486088054,-2.39624995256959,-14.3526637953744));
#11917=CARTESIAN_POINT('Ctrl Pts',(15.8,-2.33570557485288,-14.2566004799664));
#11918=CARTESIAN_POINT('',(15.8,0.328355732126618,-14.4429346149236));
#11919=CARTESIAN_POINT('Ctrl Pts',(15.8,0.328355732126618,-14.4429346149236));
#11920=CARTESIAN_POINT('Ctrl Pts',(15.7459792937636,0.322979723020245,-14.500693813047));
#11921=CARTESIAN_POINT('Ctrl Pts',(15.6927059160364,0.309313059018548,-14.5578456188156));
#11922=CARTESIAN_POINT('Ctrl Pts',(15.5867247540199,0.265397252979768,-14.6717789412864));
#11923=CARTESIAN_POINT('Ctrl Pts',(15.5350561720989,0.234952142783248,-14.7274507079622));
#11924=CARTESIAN_POINT('Ctrl Pts',(15.4151906303863,0.143523756746709,-14.856535828808));
#11925=CARTESIAN_POINT('Ctrl Pts',(15.32147738691,0.0544433185531652,-14.958098225284));
#11926=CARTESIAN_POINT('Ctrl Pts',(15.0123014953153,-0.366133555591446,
-15.2843128435264));
#11927=CARTESIAN_POINT('Ctrl Pts',(14.8382414780483,-0.667161014664403,
-15.4624487588719));
#11928=CARTESIAN_POINT('Ctrl Pts',(14.657256909085,-1.04370768816965,-15.6307858638156));
#11929=CARTESIAN_POINT('Origin',(15.8,0.,0.));
#11930=CARTESIAN_POINT('Origin',(15.75,0.,0.));
#11931=CARTESIAN_POINT('',(14.657256909085,3.83755346941362,-15.1882841634002));
#11932=CARTESIAN_POINT('',(15.8,2.18414382321291,-14.2806055031745));
#11933=CARTESIAN_POINT('Ctrl Pts',(14.657256909085,3.83755346941362,-15.1882841634002));
#11934=CARTESIAN_POINT('Ctrl Pts',(14.6761465353607,3.62787322775964,-15.220480962638));
#11935=CARTESIAN_POINT('Ctrl Pts',(14.7000757634308,3.38542345093437,-15.2500288130694));
#11936=CARTESIAN_POINT('Ctrl Pts',(14.7590833374975,3.01772165354748,-15.2622828979217));
#11937=CARTESIAN_POINT('Ctrl Pts',(14.7853594609313,2.91067193741214,-15.2539028616428));
#11938=CARTESIAN_POINT('Ctrl Pts',(14.8353557732891,2.76471831385452,-15.2268021501319));
#11939=CARTESIAN_POINT('Ctrl Pts',(14.8603859823926,2.71637224456128,-15.2082738029835));
#11940=CARTESIAN_POINT('Ctrl Pts',(14.9364214749743,2.60757230132218,-15.1451099616485));
#11941=CARTESIAN_POINT('Ctrl Pts',(14.9903198942816,2.57646607024849,-15.0921202332369));
#11942=CARTESIAN_POINT('Ctrl Pts',(15.1263879851343,2.44988270035858,-14.9660446513592));
#11943=CARTESIAN_POINT('Ctrl Pts',(15.1678275509266,2.40426863543051,-14.9286624842201));
#11944=CARTESIAN_POINT('Ctrl Pts',(15.2552258947252,2.32210737310927,-14.8473025034559));
#11945=CARTESIAN_POINT('Ctrl Pts',(15.3550596759663,2.23331369045729,-14.7532054284997));
#11946=CARTESIAN_POINT('Ctrl Pts',(15.6054597342239,2.15739979472752,-14.4945070281232));
#11947=CARTESIAN_POINT('Ctrl Pts',(15.7019486088054,2.15624789525745,-14.3906763868985));
#11948=CARTESIAN_POINT('Ctrl Pts',(15.8,2.18414382321291,-14.2806055031745));
#11949=CARTESIAN_POINT('',(15.8,4.77539710335945,-13.6345795785203));
#11950=CARTESIAN_POINT('Ctrl Pts',(15.8,4.77539710335945,-13.6345795785203));
#11951=CARTESIAN_POINT('Ctrl Pts',(15.7459792937631,4.78813278866893,-13.691173118448));
#11952=CARTESIAN_POINT('Ctrl Pts',(15.6927059160355,4.7927958980556,-13.7497509471755));
#11953=CARTESIAN_POINT('Ctrl Pts',(15.58672475402,4.78623681742324,-13.8716787063212));
#11954=CARTESIAN_POINT('Ctrl Pts',(15.535056172099,4.77448531899122,-13.9340337592382));
#11955=CARTESIAN_POINT('Ctrl Pts',(15.4151906304118,4.7274212527491,-14.0850539295969));
#11956=CARTESIAN_POINT('Ctrl Pts',(15.3214773869328,4.67408522804331,-14.2091728778437));
#11957=CARTESIAN_POINT('Ctrl Pts',(15.0123014953203,4.37489871211817,-14.649386817811));
#11958=CARTESIAN_POINT('Ctrl Pts',(14.8382414780549,4.14365161073977,-14.9118267415107));
#11959=CARTESIAN_POINT('Ctrl Pts',(14.657256909085,3.83755346941362,-15.1882841634002));
#11960=CARTESIAN_POINT('Origin',(15.8,0.,0.));
#11961=CARTESIAN_POINT('Origin',(15.75,0.,0.));
#11962=CARTESIAN_POINT('',(14.657256909085,8.34316815560344,-13.2590473860729));
#11963=CARTESIAN_POINT('',(15.8,6.49019400603777,-12.9067253609027));
#11964=CARTESIAN_POINT('Ctrl Pts',(14.657256909085,8.34316815560344,-13.2590473860729));
#11965=CARTESIAN_POINT('Ctrl Pts',(14.6761465353606,8.15369975356969,-13.3544631198472));
#11966=CARTESIAN_POINT('Ctrl Pts',(14.7000757634305,7.93224710137849,-13.4574858968629));
#11967=CARTESIAN_POINT('Ctrl Pts',(14.7590833374994,7.58632863137506,-13.5827663283737));
#11968=CARTESIAN_POINT('Ctrl Pts',(14.7853594609344,7.48192872765686,-13.6078766217891));
#11969=CARTESIAN_POINT('Ctrl Pts',(14.8353557732885,7.33474400248902,-13.6272044635792));
#11970=CARTESIAN_POINT('Ctrl Pts',(14.860385982392,7.2830385841035,-13.6245227153106));
#11971=CARTESIAN_POINT('Ctrl Pts',(14.936421474974,7.16004498871036,-13.5980713638626));
#11972=CARTESIAN_POINT('Ctrl Pts',(14.99031989428,7.11408647834531,-13.5572874913936));
#11973=CARTESIAN_POINT('Ctrl Pts',(15.1263879851359,6.95473904217717,-13.4764989002024));
#11974=CARTESIAN_POINT('Ctrl Pts',(15.1678275509259,6.89980576356277,-13.4550418677983));
#11975=CARTESIAN_POINT('Ctrl Pts',(15.2552258947264,6.79652414292473,-13.4030531542622));
#11976=CARTESIAN_POINT('Ctrl Pts',(15.3550596759669,6.6829987371513,-13.3410002748937));
#11977=CARTESIAN_POINT('Ctrl Pts',(15.6054597342247,6.5308581298062,-13.1184221593499));
#11978=CARTESIAN_POINT('Ctrl Pts',(15.7019486088066,6.49767717563412,-13.0200293079335));
#11979=CARTESIAN_POINT('Ctrl Pts',(15.8,6.49019400603777,-12.9067253609027));
#11980=CARTESIAN_POINT('',(15.8,8.7549893339674,-11.4915768952696));
#11981=CARTESIAN_POINT('Ctrl Pts',(15.8,8.7549893339674,-11.4915768952696));
#11982=CARTESIAN_POINT('Ctrl Pts',(15.7459792937641,8.78459005607935,-11.5414650070014));
#11983=CARTESIAN_POINT('Ctrl Pts',(15.6927059160371,8.80712648121827,-11.5957348526753));
#11984=CARTESIAN_POINT('Ctrl Pts',(15.5867247540197,8.83856617450453,-11.7137219099129));
#11985=CARTESIAN_POINT('Ctrl Pts',(15.5350561720989,8.84665860638097,-11.7766565020382));
#11986=CARTESIAN_POINT('Ctrl Pts',(15.4151906304187,8.8485658186322,-11.9348288154339));
#11987=CARTESIAN_POINT('Ctrl Pts',(15.3214773869393,8.83619510911792,-12.0693546880046));
#11988=CARTESIAN_POINT('Ctrl Pts',(15.0123014953214,8.6876854121677,-12.5804767420922));
#11989=CARTESIAN_POINT('Ctrl Pts',(14.8382414780552,8.54885474595289,-12.9015312258898));
#11990=CARTESIAN_POINT('Ctrl Pts',(14.657256909085,8.34316815560344,-13.2590473860729));
#11991=CARTESIAN_POINT('Origin',(15.8,0.,0.));
#11992=CARTESIAN_POINT('Origin',(15.75,0.,0.));
#11993=CARTESIAN_POINT('',(14.657256909085,12.0320954124521,-10.0319226693815));
#11994=CARTESIAN_POINT('',(15.8,10.160938779711,-10.2694450138623));
#11995=CARTESIAN_POINT('Ctrl Pts',(14.657256909085,12.0320954124521,-10.0319226693815));
#11996=CARTESIAN_POINT('Ctrl Pts',(14.6761465353605,11.881385337334,-10.181217380869));
#11997=CARTESIAN_POINT('Ctrl Pts',(14.7000757634302,11.7026071383233,-10.3476304972523));
#11998=CARTESIAN_POINT('Ctrl Pts',(14.759083337498,11.4123329057235,-10.5736739539013));
#11999=CARTESIAN_POINT('Ctrl Pts',(14.7853594609327,11.320802204389,-10.6298166065426));
#12000=CARTESIAN_POINT('Ctrl Pts',(14.8353557732875,11.1867938439948,-10.6936810578134));
#12001=CARTESIAN_POINT('Ctrl Pts',(14.8603859823904,11.1367903631218,-10.7071084166307));
#12002=CARTESIAN_POINT('Ctrl Pts',(14.9364214749737,11.0116425856365,-10.7199587976476));
#12003=CARTESIAN_POINT('Ctrl Pts',(14.9903198942803,10.9553305351849,-10.6953729907148));
#12004=CARTESIAN_POINT('Ctrl Pts',(15.1263879851363,10.7788170700321,-10.6677795404063));
#12005=CARTESIAN_POINT('Ctrl Pts',(15.1678275509267,10.7199418297822,-10.6643480065664));
#12006=CARTESIAN_POINT('Ctrl Pts',(15.2552258947248,10.6056497754659,-10.6468195777683));
#12007=CARTESIAN_POINT('Ctrl Pts',(15.3550596759664,10.4785053042635,-10.6228850621674));
#12008=CARTESIAN_POINT('Ctrl Pts',(15.6054597342242,10.2650305679759,-10.4582147281989));
#12009=CARTESIAN_POINT('Ctrl Pts',(15.7019486088058,10.2030685420808,-10.3748910444316));
#12010=CARTESIAN_POINT('Ctrl Pts',(15.8,10.160938779711,-10.2694450138623));
#12011=CARTESIAN_POINT('',(15.8,11.8775822089691,-8.22369859898568));
#12012=CARTESIAN_POINT('Ctrl Pts',(15.8,11.8775822089691,-8.22369859898568));
#12013=CARTESIAN_POINT('Ctrl Pts',(15.7459792937641,11.9211504429631,-8.26199788655548));
#12014=CARTESIAN_POINT('Ctrl Pts',(15.6927059160372,11.9593541615407,-8.30664743856149));
#12015=CARTESIAN_POINT('Ctrl Pts',(15.5867247540198,12.0257150925137,-8.40914439866246));
#12016=CARTESIAN_POINT('Ctrl Pts',(15.535056172099,12.0528593110832,-8.46649805362797));
#12017=CARTESIAN_POINT('Ctrl Pts',(15.4151906304144,12.1035511106034,-8.61633950198822));
#12018=CARTESIAN_POINT('Ctrl Pts',(15.3214773869356,12.1333566475145,-8.74810396918045));
#12019=CARTESIAN_POINT('Ctrl Pts',(15.0123014953203,12.1500609334098,-9.28010194952505));
#12020=CARTESIAN_POINT('Ctrl Pts',(14.8382414780551,12.1172364152582,-9.62834394362577));
#12021=CARTESIAN_POINT('Ctrl Pts',(14.657256909085,12.0320954124521,-10.0319226693815));
#12022=CARTESIAN_POINT('Origin',(15.8,0.,0.));
#12023=CARTESIAN_POINT('Origin',(15.75,0.,0.));
#12024=CARTESIAN_POINT('',(14.657256909085,14.5432373377918,-5.82280346529581));
#12025=CARTESIAN_POINT('',(15.8,12.8370600702028,-6.62691983743441));
#12026=CARTESIAN_POINT('Ctrl Pts',(14.657256909085,14.5432373377918,-5.82280346529581));
#12027=CARTESIAN_POINT('Ctrl Pts',(14.6761465353606,14.4460381417986,-6.01136314794077));
#12028=CARTESIAN_POINT('Ctrl Pts',(14.7000757634307,14.3274344517053,-6.22487692839559));
#12029=CARTESIAN_POINT('Ctrl Pts',(14.7590833374967,14.1212185208583,-6.52955670169685));
#12030=CARTESIAN_POINT('Ctrl Pts',(14.7853594609302,14.0515166846884,-6.6112360795567));
#12031=CARTESIAN_POINT('Ctrl Pts',(14.8353557732895,13.9438023610675,-6.7133856428557));
#12032=CARTESIAN_POINT('Ctrl Pts',(14.8603859823933,13.9003955068096,-6.74160774532172));
#12033=CARTESIAN_POINT('Ctrl Pts',(14.9364214749747,13.7853438836539,-6.7925019739738));
#12034=CARTESIAN_POINT('Ctrl Pts',(14.9903198942819,13.7241905089622,-6.78652086266021));
#12035=CARTESIAN_POINT('Ctrl Pts',(15.1263879851332,13.5477893826425,-6.81482359240399));
#12036=CARTESIAN_POINT('Ctrl Pts',(15.1678275509259,13.4907352994781,-6.82975345957037));
#12037=CARTESIAN_POINT('Ctrl Pts',(15.2552258947254,13.3766205140745,-6.8484011202478));
#12038=CARTESIAN_POINT('Ctrl Pts',(15.3550596759662,13.2483027641548,-6.86492784556321));
#12039=CARTESIAN_POINT('Ctrl Pts',(15.6054597342237,12.9943902934786,-6.77428437278497));
#12040=CARTESIAN_POINT('Ctrl Pts',(15.7019486088047,12.9097124706706,-6.71418615938453));
#12041=CARTESIAN_POINT('Ctrl Pts',(15.8,12.8370600702028,-6.62691983743441));
#12042=CARTESIAN_POINT('',(15.8,13.8375145813754,-4.15082738595569));
#12043=CARTESIAN_POINT('Ctrl Pts',(15.8,13.8375145813754,-4.15082738595568));
#12044=CARTESIAN_POINT('Ctrl Pts',(15.7459792937632,13.8907855649513,-4.17378884824973));
#12045=CARTESIAN_POINT('Ctrl Pts',(15.6927059160362,13.9409169308123,-4.2044474973462));
#12046=CARTESIAN_POINT('Ctrl Pts',(15.5867247540197,14.0357032291838,-4.28142124371687));
#12047=CARTESIAN_POINT('Ctrl Pts',(15.5350561720987,14.0792421692081,-4.32757978616837));
#12048=CARTESIAN_POINT('Ctrl Pts',(15.41519063041,14.1737564894728,-4.45442284451972));
#12049=CARTESIAN_POINT('Ctrl Pts',(15.3214773869312,14.24282069919,-4.57052788222937));
#12050=CARTESIAN_POINT('Ctrl Pts',(15.01230149532,14.423103836038,-5.07132611986488));
#12051=CARTESIAN_POINT('Ctrl Pts',(14.8382414780537,14.499498558488,-5.4126672715457));
#12052=CARTESIAN_POINT('Ctrl Pts',(14.657256909085,14.5432373377918,-5.82280346529581));
#12053=CARTESIAN_POINT('Origin',(15.8,0.,0.));
#12054=CARTESIAN_POINT('Origin',(15.75,0.,0.));
#12055=CARTESIAN_POINT('',(15.8218384638272,-14.4233723052509,1.76635367265361E-15));
#12056=CARTESIAN_POINT('Origin',(15.8218384638272,0.,0.));
#12057=CARTESIAN_POINT('',(19.5,-10.5,-1.28587913910472E-15));
#12058=CARTESIAN_POINT('',(15.75,-14.5,-1.77573785876366E-15));
#12059=CARTESIAN_POINT('Origin',(19.5,0.,0.));
#12060=CARTESIAN_POINT('Origin',(21.25,0.,0.));
#12061=CARTESIAN_POINT('',(21.,-10.5,-1.28587913910472E-15));
#12062=CARTESIAN_POINT('',(21.25,-10.5,-1.28587913910472E-15));
#12063=CARTESIAN_POINT('Origin',(21.,0.,0.));
#12064=CARTESIAN_POINT('Origin',(15.75,0.,0.));
#12065=CARTESIAN_POINT('',(14.657256909085,15.6307858638156,-1.04370768816965));
#12066=CARTESIAN_POINT('',(15.8,14.2566004799664,-2.33570557485288));
#12067=CARTESIAN_POINT('Ctrl Pts',(14.657256909085,15.6307858638156,-1.04370768816965));
#12068=CARTESIAN_POINT('Ctrl Pts',(14.6761465353607,15.5966120814788,-1.25307480646179));
#12069=CARTESIAN_POINT('Ctrl Pts',(14.7000757634308,15.5497926558527,-1.49278903451664));
#12070=CARTESIAN_POINT('Ctrl Pts',(14.7590833374963,15.4478208788501,-1.84628094543702));
#12071=CARTESIAN_POINT('Ctrl Pts',(14.7853594609294,15.406770809212,-1.94550170191398));
#12072=CARTESIAN_POINT('Ctrl Pts',(14.8353557732901,15.3358943508592,-2.07593726626672));
#12073=CARTESIAN_POINT('Ctrl Pts',(14.8603859823943,15.3033330885441,-2.11619153635774));
#12074=CARTESIAN_POINT('Ctrl Pts',(14.9364214749742,15.2096396742025,-2.20014773094342));
#12075=CARTESIAN_POINT('Ctrl Pts',(14.9903198942812,15.1496310936677,-2.2133567880967));
#12076=CARTESIAN_POINT('Ctrl Pts',(15.1263879851347,14.9906096774748,-2.29478522950976));
#12077=CARTESIAN_POINT('Ctrl Pts',(15.1678275509265,14.9409616025794,-2.32661505826142));
#12078=CARTESIAN_POINT('Ctrl Pts',(15.2552258947252,14.8381944363711,-2.37961344546101));
#12079=CARTESIAN_POINT('Ctrl Pts',(15.3550596759664,14.7212640431372,-2.43498366067061));
#12080=CARTESIAN_POINT('Ctrl Pts',(15.6054597342241,14.4517685598141,-2.42723986374772));
#12081=CARTESIAN_POINT('Ctrl Pts',(15.7019486088057,14.352663795374,-2.39624995256937));
#12082=CARTESIAN_POINT('Ctrl Pts',(15.8,14.2566004799664,-2.33570557485288));
#12083=CARTESIAN_POINT('',(15.8,14.4429346149236,0.328355732126616));
#12084=CARTESIAN_POINT('Ctrl Pts',(15.8,14.4429346149236,0.328355732126617));
#12085=CARTESIAN_POINT('Ctrl Pts',(15.7459792937636,14.500693813047,0.322979723020245));
#12086=CARTESIAN_POINT('Ctrl Pts',(15.6927059160366,14.5578456188153,0.309313059018634));
#12087=CARTESIAN_POINT('Ctrl Pts',(15.5867247540197,14.6717789412866,0.265397252979699));
#12088=CARTESIAN_POINT('Ctrl Pts',(15.5350561720988,14.7274507079623,0.234952142783187));
#12089=CARTESIAN_POINT('Ctrl Pts',(15.415190630386,14.8565358288083,0.143523756746544));
#12090=CARTESIAN_POINT('Ctrl Pts',(15.3214773869099,14.9580982252841,0.0544433185530627));
#12091=CARTESIAN_POINT('Ctrl Pts',(15.0123014953152,15.2843128435265,-0.366133555591651));
#12092=CARTESIAN_POINT('Ctrl Pts',(14.8382414780497,15.4624487588706,-0.667161014661462));
#12093=CARTESIAN_POINT('Ctrl Pts',(14.657256909085,15.6307858638156,-1.04370768816965));
#12094=CARTESIAN_POINT('Origin',(15.8,0.,0.));
#12095=CARTESIAN_POINT('Ctrl Pts',(10.0502525316942,9.05620683581208,-1.38781479615277));
#12096=CARTESIAN_POINT('Ctrl Pts',(11.9668350211294,10.8374137839212,-0.817330781359225));
#12097=CARTESIAN_POINT('Ctrl Pts',(13.8834175105647,12.6186207320302,-0.246846766565678));
#12098=CARTESIAN_POINT('Ctrl Pts',(15.8,14.3998276801393,0.323637248227868));
#12099=CARTESIAN_POINT('Ctrl Pts',(10.0502525316942,9.21244502400637,-1.39655842853149));
#12100=CARTESIAN_POINT('Ctrl Pts',(11.9668350211294,11.0233696506194,-0.813302761662289));
#12101=CARTESIAN_POINT('Ctrl Pts',(13.8834175105647,12.8346197703481,-0.230291956370556));
#12102=CARTESIAN_POINT('Ctrl Pts',(15.8,14.6455443969612,0.352963710498642));
#12103=CARTESIAN_POINT('Ctrl Pts',(10.0502525316942,9.51829373400973,-1.46541714813614));
#12104=CARTESIAN_POINT('Ctrl Pts',(11.9668350211295,11.3925515672309,-0.867231464171977));
#12105=CARTESIAN_POINT('Ctrl Pts',(13.8834175105647,13.2668740653714,-0.269566015193986));
#12106=CARTESIAN_POINT('Ctrl Pts',(15.8,15.1411318985925,0.328619668770177));
#12107=CARTESIAN_POINT('Ctrl Pts',(10.0502525316941,10.0083300006652,-1.79039750449509));
#12108=CARTESIAN_POINT('Ctrl Pts',(11.9668350211294,12.0019243797287,-1.20809631886684));
#12109=CARTESIAN_POINT('Ctrl Pts',(13.8834175105647,13.9956114385883,-0.625444427693875));
#12110=CARTESIAN_POINT('Ctrl Pts',(15.7999999999999,15.9892058176519,-0.0431432420656254));
#12111=CARTESIAN_POINT('Ctrl Pts',(10.0502525316942,10.3276659549724,-2.10732113862254));
#12112=CARTESIAN_POINT('Ctrl Pts',(11.9668350211294,12.4074689224609,-1.55295659524518));
#12113=CARTESIAN_POINT('Ctrl Pts',(13.8834175105647,14.4874157824202,-0.999648742962752));
#12114=CARTESIAN_POINT('Ctrl Pts',(15.8,16.5672187499087,-0.445284199585385));
#12115=CARTESIAN_POINT('Ctrl Pts',(10.0502525316942,10.5073910450885,-2.3220627978979));
#12116=CARTESIAN_POINT('Ctrl Pts',(11.9668350211294,12.6387996550358,-1.79024801807933));
#12117=CARTESIAN_POINT('Ctrl Pts',(13.8834175105647,14.7702082649831,-1.25843323826077));
#12118=CARTESIAN_POINT('Ctrl Pts',(15.8,16.9016168749304,-0.726618458442204));
#12119=CARTESIAN_POINT('',(10.0502525316942,10.5073910450885,-2.3220627978979));
#12120=CARTESIAN_POINT('',(15.8,14.3998276801393,0.323637248227868));
#12121=CARTESIAN_POINT('Ctrl Pts',(15.8,14.3998276801393,0.323637248227868));
#12122=CARTESIAN_POINT('Ctrl Pts',(15.5456570571831,14.1695921802544,0.248663394075437));
#12123=CARTESIAN_POINT('Ctrl Pts',(15.2905259507727,13.9381981568648,0.173284602940039));
#12124=CARTESIAN_POINT('Ctrl Pts',(15.0353275664552,13.7061319160866,0.097716587704992));
#12125=CARTESIAN_POINT('Ctrl Pts',(14.7778789011692,13.4720193682894,0.0214822310000918));
#12126=CARTESIAN_POINT('Ctrl Pts',(14.5203617662627,13.2372226466704,-0.0549444640635663));
#12127=CARTESIAN_POINT('Ctrl Pts',(14.2635162858846,13.0022894235192,-0.131318796804586));
#12128=CARTESIAN_POINT('Ctrl Pts',(14.0000820510511,12.7613295522894,-0.209652329779127));
#12129=CARTESIAN_POINT('Ctrl Pts',(13.7373543721026,12.5202260255194,-0.287930509546324));
#12130=CARTESIAN_POINT('Ctrl Pts',(13.4761318051383,12.2796215208074,-0.365868800886744));
#12131=CARTESIAN_POINT('Ctrl Pts',(13.2939592679836,12.1118276981541,-0.420221747647761));
#12132=CARTESIAN_POINT('Ctrl Pts',(13.1125187344709,11.9442776868953,-0.474408950394494));
#12133=CARTESIAN_POINT('Ctrl Pts',(12.9320810503802,11.7772036867065,-0.528329405335829));
#12134=CARTESIAN_POINT('Ctrl Pts',(12.7419408368636,11.6011457516413,-0.585149281223285));
#12135=CARTESIAN_POINT('Ctrl Pts',(12.5505198646271,11.4234544410918,-0.642388101081205));
#12136=CARTESIAN_POINT('Ctrl Pts',(12.3584606652983,11.2445392798298,-0.699829652727959));
#12137=CARTESIAN_POINT('Ctrl Pts',(12.1609507027362,11.0605463915632,-0.758901432444389));
#12138=CARTESIAN_POINT('Ctrl Pts',(11.9627657724266,10.8752590885173,-0.818187336020626));
#12139=CARTESIAN_POINT('Ctrl Pts',(11.7646046796663,10.6891763370134,-0.877435109077808));
#12140=CARTESIAN_POINT('Ctrl Pts',(11.5611733354013,10.4981445670748,-0.938258623673124));
#12141=CARTESIAN_POINT('Ctrl Pts',(11.3577671135037,10.3062745975188,-0.999041534288636));
#12142=CARTESIAN_POINT('Ctrl Pts',(11.1551420711314,10.1141619588695,-1.05949856916707));
#12143=CARTESIAN_POINT('Ctrl Pts',(10.9369470578885,9.90728713607633,-1.12460120096165));
#12144=CARTESIAN_POINT('Ctrl Pts',(10.7196578904059,9.70013097729891,-1.18932539513645));
#12145=CARTESIAN_POINT('Ctrl Pts',(10.5042186507229,9.49350036754279,-1.25330845309519));
#12146=CARTESIAN_POINT('Ctrl Pts',(10.3518600992381,9.34737127591962,-1.29855724827523));
#12147=CARTESIAN_POINT('Ctrl Pts',(10.2004267545904,9.20150648816192,-1.34343522942928));
#12148=CARTESIAN_POINT('Ctrl Pts',(10.0502525316942,9.05620683581208,-1.38781479615277));
#12149=CARTESIAN_POINT('Ctrl Pts',(15.8,14.3998276801393,0.323637248227868));
#12150=CARTESIAN_POINT('Ctrl Pts',(15.8,14.4084472574799,0.324666000821255));
#12151=CARTESIAN_POINT('Ctrl Pts',(15.8,14.4170677396245,0.325652230376826));
#12152=CARTESIAN_POINT('Ctrl Pts',(15.8,14.4256891265865,0.326595936941114));
#12153=CARTESIAN_POINT('Ctrl Pts',(15.8,14.434311418564,0.327497110819206));
#12154=CARTESIAN_POINT('Ctrl Pts',(15.8,14.4429346149236,0.328355732126616));
#12155=CARTESIAN_POINT('Ctrl Pts',(10.0502525316942,8.18410616705958,-4.11841212213243));
#12156=CARTESIAN_POINT('Ctrl Pts',(11.9668350211294,10.0544238975194,-4.12627279988524));
#12157=CARTESIAN_POINT('Ctrl Pts',(13.8834175105647,11.9247416279792,-4.13413347763806));
#12158=CARTESIAN_POINT('Ctrl Pts',(15.8,13.795059358439,-4.14199415539088));
#12159=CARTESIAN_POINT('Ctrl Pts',(10.0502525316942,8.32999558303832,-4.17500806600468));
#12160=CARTESIAN_POINT('Ctrl Pts',(11.9668350211294,10.2325231628261,-4.17990544851819));
#12161=CARTESIAN_POINT('Ctrl Pts',(13.8834175105647,12.1352846385738,-4.18513629113481));
#12162=CARTESIAN_POINT('Ctrl Pts',(15.8,14.0378122183616,-4.19003367364832));
#12163=CARTESIAN_POINT('Ctrl Pts',(10.0502525316942,8.59959242261693,-4.33502367302148));
#12164=CARTESIAN_POINT('Ctrl Pts',(11.9668350211294,10.5669670902559,-4.34529280263859));
#12165=CARTESIAN_POINT('Ctrl Pts',(13.8834175105647,12.5342444956752,-4.35608887336511));
#12166=CARTESIAN_POINT('Ctrl Pts',(15.8,14.5016191633141,-4.36635800298221));
#12167=CARTESIAN_POINT('Ctrl Pts',(10.0502525316941,8.9652188127798,-4.79552866926094));
#12168=CARTESIAN_POINT('Ctrl Pts',(11.9668350211294,11.0411807000414,-4.85778187524381));
#12169=CARTESIAN_POINT('Ctrl Pts',(13.8834175105647,13.1173407686982,-4.91974349130657));
#12170=CARTESIAN_POINT('Ctrl Pts',(15.7999999999999,15.1933026559598,-4.98199669728944));
#12171=CARTESIAN_POINT('Ctrl Pts',(10.0502525316942,9.17099596015618,-5.19560579312752));
#12172=CARTESIAN_POINT('Ctrl Pts',(11.9668350211294,11.3203141899786,-5.31106824365088));
#12173=CARTESIAN_POINT('Ctrl Pts',(13.8834175105647,13.469442734167,-5.42758013234469));
#12174=CARTESIAN_POINT('Ctrl Pts',(15.8,15.6187609639894,-5.54304258286805));
#12175=CARTESIAN_POINT('Ctrl Pts',(10.0502525316942,9.2755658561365,-5.45537535466284));
#12176=CARTESIAN_POINT('Ctrl Pts',(11.9668350211294,11.4669957083382,-5.60823092528513));
#12177=CARTESIAN_POINT('Ctrl Pts',(13.8834175105647,13.6584255605399,-5.76108649590741));
#12178=CARTESIAN_POINT('Ctrl Pts',(15.8,15.8498554127416,-5.91394206652969));
#12179=CARTESIAN_POINT('',(10.0502525316942,9.2755658561365,-5.45537535466284));
#12180=CARTESIAN_POINT('',(15.8,13.795059358439,-4.14199415539088));
#12181=CARTESIAN_POINT('Ctrl Pts',(15.8,13.795059358439,-4.14199415539088));
#12182=CARTESIAN_POINT('Ctrl Pts',(15.5456574794168,13.5529245928917,-4.14215184549968));
#12183=CARTESIAN_POINT('Ctrl Pts',(15.290526797857,13.3095628770617,-4.14233665870497));
#12184=CARTESIAN_POINT('Ctrl Pts',(15.0353288374168,13.0655033718493,-4.14249371366664));
#12185=CARTESIAN_POINT('Ctrl Pts',(14.7778805061944,12.8192917162879,-4.1426521535606));
#12186=CARTESIAN_POINT('Ctrl Pts',(14.5203637043112,12.5723699372145,-4.14278210218064));
#12187=CARTESIAN_POINT('Ctrl Pts',(14.263518553037,12.3253345162712,-4.14282007025482));
#12188=CARTESIAN_POINT('Ctrl Pts',(14.0000848089524,12.0719621417578,-4.14285901228618));
#12189=CARTESIAN_POINT('Ctrl Pts',(13.7373576158079,11.8184702457672,-4.14280091850188));
#12190=CARTESIAN_POINT('Ctrl Pts',(13.4761355252029,11.5655579735774,-4.14257377376942));
#12191=CARTESIAN_POINT('Ctrl Pts',(13.2939617380614,11.3891793743071,-4.14241536520586));
#12192=CARTESIAN_POINT('Ctrl Pts',(13.1125199626835,11.2130838733106,-4.14217466317553));
#12193=CARTESIAN_POINT('Ctrl Pts',(12.9320810503802,11.0375235228707,-4.14182735974364));
#12194=CARTESIAN_POINT('Ctrl Pts',(12.7419408575526,10.8525241873095,-4.14146138357661));
#12195=CARTESIAN_POINT('Ctrl Pts',(12.5505199062838,10.6658419590985,-4.14098910290385));
#12196=CARTESIAN_POINT('Ctrl Pts',(12.3584607279918,10.4779331330927,-4.14033143664814));
#12197=CARTESIAN_POINT('Ctrl Pts',(12.1609502835644,10.2846908414914,-4.13965510367823));
#12198=CARTESIAN_POINT('Ctrl Pts',(11.9627648680213,10.0901513147852,-4.13878241284077));
#12199=CARTESIAN_POINT('Ctrl Pts',(11.7646032917752,9.89486705365802,-4.13762764472381));
#12200=CARTESIAN_POINT('Ctrl Pts',(11.5611710263525,9.69438863400127,-4.1364421621569));
#12201=CARTESIAN_POINT('Ctrl Pts',(11.3577638852442,9.4931255822132,-4.13495903745938));
#12202=CARTESIAN_POINT('Ctrl Pts',(11.1551379358798,9.29173244419996,-4.13309099161787));
#12203=CARTESIAN_POINT('Ctrl Pts',(10.9369434970433,9.07486553809952,-4.13107941701262));
#12204=CARTESIAN_POINT('Ctrl Pts',(10.7196549052569,8.85784801697106,-4.1286209883191));
#12205=CARTESIAN_POINT('Ctrl Pts',(10.5042162352524,8.64155934492939,-4.1256201089363));
#12206=CARTESIAN_POINT('Ctrl Pts',(10.3518584987032,8.4886004888762,-4.1234978938743));
#12207=CARTESIAN_POINT('Ctrl Pts',(10.2004259609769,8.33600758581753,-4.12110469363328));
#12208=CARTESIAN_POINT('Ctrl Pts',(10.0502525316942,8.18410616705958,-4.11841212213243));
#12209=CARTESIAN_POINT('Ctrl Pts',(15.8,13.795059358439,-4.14199415539088));
#12210=CARTESIAN_POINT('Ctrl Pts',(15.8,13.8035749656708,-4.14367934941586));
#12211=CARTESIAN_POINT('Ctrl Pts',(15.8,13.8120782930811,-4.14540526485286));
#12212=CARTESIAN_POINT('Ctrl Pts',(15.8,13.8205693406969,-4.14717190166177));
#12213=CARTESIAN_POINT('Ctrl Pts',(15.8,13.8290481057107,-4.14897926912419));
#12214=CARTESIAN_POINT('Ctrl Pts',(15.8,13.8375145813754,-4.15082738595568));
#12215=CARTESIAN_POINT('Ctrl Pts',(10.0502525316942,6.51088816465465,-6.44587057493322));
#12216=CARTESIAN_POINT('Ctrl Pts',(11.9668350211294,8.28723694673789,-7.03130648732539));
#12217=CARTESIAN_POINT('Ctrl Pts',(13.8834175105647,10.0635857288211,-7.61674239971757));
#12218=CARTESIAN_POINT('Ctrl Pts',(15.8,11.8399345109044,-8.20217831210975));
#12219=CARTESIAN_POINT('Ctrl Pts',(10.0502525316942,6.63214813591051,-6.54477882498566));
#12220=CARTESIAN_POINT('Ctrl Pts',(11.9668350211294,8.4400460136743,-7.13734986695939));
#12221=CARTESIAN_POINT('Ctrl Pts',(13.8834175105647,10.2480632948761,-7.73031032616364));
#12222=CARTESIAN_POINT('Ctrl Pts',(15.8,12.0559611726399,-8.32288136813736));
#12223=CARTESIAN_POINT('Ctrl Pts',(10.0502525316942,6.83909882511011,-6.78027814405441));
#12224=CARTESIAN_POINT('Ctrl Pts',(11.9668350211295,8.70700998719299,-7.39799687329663));
#12225=CARTESIAN_POINT('Ctrl Pts',(13.8834175105647,10.5746650104356,-8.0161919374395));
#12226=CARTESIAN_POINT('Ctrl Pts',(15.8,12.4425761725185,-8.63391066668172));
#12227=CARTESIAN_POINT('Ctrl Pts',(10.0502525316941,7.04452561799898,-7.33122941665118));
#12228=CARTESIAN_POINT('Ctrl Pts',(11.9668350211294,8.99964539985649,-8.03194323669998));
#12229=CARTESIAN_POINT('Ctrl Pts',(13.8834175105647,10.9550426722923,-8.73244671395171));
#12230=CARTESIAN_POINT('Ctrl Pts',(15.8,12.9101624541498,-9.43316053400051));
#12231=CARTESIAN_POINT('Ctrl Pts',(10.0502525316942,7.11660498267375,-7.77530835268703));
#12232=CARTESIAN_POINT('Ctrl Pts',(11.9668350211294,9.12504823131445,-8.54929552797968));
#12233=CARTESIAN_POINT('Ctrl Pts',(13.8834175105647,11.1329867839676,-9.32422216219827));
#12234=CARTESIAN_POINT('Ctrl Pts',(15.8,13.1414300326083,-10.0982093374909));
#12235=CARTESIAN_POINT('Ctrl Pts',(10.0502525316942,7.13578365451837,-8.05467776187827));
#12236=CARTESIAN_POINT('Ctrl Pts',(11.9668350211294,9.17272232645135,-8.8772411146815));
#12237=CARTESIAN_POINT('Ctrl Pts',(13.8834175105647,11.2096609983843,-9.69980446748474));
#12238=CARTESIAN_POINT('Ctrl Pts',(15.8,13.2465996703173,-10.522367820288));
#12239=CARTESIAN_POINT('',(10.0502525316942,7.13578365451837,-8.05467776187827));
#12240=CARTESIAN_POINT('',(15.8,11.8399345109044,-8.20217831210975));
#12241=CARTESIAN_POINT('Ctrl Pts',(15.8,11.8399345109044,-8.20217831210975));
#12242=CARTESIAN_POINT('Ctrl Pts',(15.5456576615067,11.6096021002861,-8.12750458029291));
#12243=CARTESIAN_POINT('Ctrl Pts',(15.2905271631653,11.3780944093848,-8.05247749955188));
#12244=CARTESIAN_POINT('Ctrl Pts',(15.0353293855237,11.1459316587091,-7.97720839274425));
#12245=CARTESIAN_POINT('Ctrl Pts',(14.7778811978195,10.9117216277039,-7.90127554051952));
#12246=CARTESIAN_POINT('Ctrl Pts',(14.5203645390055,10.6768450327867,-7.82509615349673));
#12247=CARTESIAN_POINT('Ctrl Pts',(14.2635195291145,10.4418887807062,-7.748794170348));
#12248=CARTESIAN_POINT('Ctrl Pts',(14.0000859949211,10.2009054892938,-7.67053490770798));
#12249=CARTESIAN_POINT('Ctrl Pts',(13.7373590095462,9.95983851106089,-7.59214642417434));
#12250=CARTESIAN_POINT('Ctrl Pts',(13.4761371226647,9.71937502567175,-7.51377627479589));
#12251=CARTESIAN_POINT('Ctrl Pts',(13.2939627987566,9.5516774663351,-7.45912147864526));
#12252=CARTESIAN_POINT('Ctrl Pts',(13.1125204900998,9.38427458086322,-7.404475897828));
#12253=CARTESIAN_POINT('Ctrl Pts',(12.9320810503802,9.21741359915303,-7.34989430276011));
#12254=CARTESIAN_POINT('Ctrl Pts',(12.7419408661181,9.0415818749035,-7.29237830426415));
#12255=CARTESIAN_POINT('Ctrl Pts',(12.5505199235302,8.8641824751674,-7.23424116054649));
#12256=CARTESIAN_POINT('Ctrl Pts',(12.3584607539476,8.68567379986616,-7.17554866346896));
#12257=CARTESIAN_POINT('Ctrl Pts',(12.1609501017811,8.5020982645104,-7.11519021559973));
#12258=CARTESIAN_POINT('Ctrl Pts',(11.9627644770481,8.31734966162794,-7.0542441495787));
#12259=CARTESIAN_POINT('Ctrl Pts',(11.7646026923668,8.13197994128604,-6.99279967398786));
#12260=CARTESIAN_POINT('Ctrl Pts',(11.5611700299521,7.9416795975498,-6.92972084534173));
#12261=CARTESIAN_POINT('Ctrl Pts',(11.3577624926924,7.75072500004993,-6.86611647390364));
#12262=CARTESIAN_POINT('Ctrl Pts',(11.1551361524442,7.55976563308339,-6.80210582000275));
#12263=CARTESIAN_POINT('Ctrl Pts',(10.9369419552394,7.35413478704945,-6.73317720379544));
#12264=CARTESIAN_POINT('Ctrl Pts',(10.7196536056915,7.1484987864115,-6.66377706212351));
#12265=CARTESIAN_POINT('Ctrl Pts',(10.5042151754601,6.94372358733477,-6.5940862490785));
#12266=CARTESIAN_POINT('Ctrl Pts',(10.3518577964654,6.79890721181192,-6.54480112569479));
#12267=CARTESIAN_POINT('Ctrl Pts',(10.2004256127774,6.65452261540791,-6.49537136769534));
#12268=CARTESIAN_POINT('Ctrl Pts',(10.0502525316942,6.51088816465465,-6.44587057493322));
#12269=CARTESIAN_POINT('Ctrl Pts',(15.8,11.8399345109044,-8.20217831210975));
#12270=CARTESIAN_POINT('Ctrl Pts',(15.8,11.8475125810599,-8.20641249422049));
#12271=CARTESIAN_POINT('Ctrl Pts',(15.8,11.8550663888027,-8.21068161002192));
#12272=CARTESIAN_POINT('Ctrl Pts',(15.8,11.862595934171,-8.21498565948429));
#12273=CARTESIAN_POINT('Ctrl Pts',(15.8,11.8701012116266,-8.21932465056733));
#12274=CARTESIAN_POINT('Ctrl Pts',(15.8,11.8775822089691,-8.22369859898568));
#12275=CARTESIAN_POINT('Ctrl Pts',(10.0502525316942,4.20033906466803,-8.14236230483842));
#12276=CARTESIAN_POINT('Ctrl Pts',(11.9668350211294,5.70883750303466,-9.24806690579316));
#12277=CARTESIAN_POINT('Ctrl Pts',(13.8834175105647,7.21733594140129,-10.3537715067479));
#12278=CARTESIAN_POINT('Ctrl Pts',(15.8,8.72583437976793,-11.4594761077026));
#12279=CARTESIAN_POINT('Ctrl Pts',(10.0502525316942,4.28509982034658,-8.27390103242161));
#12280=CARTESIAN_POINT('Ctrl Pts',(11.9668350211294,5.82139835544565,-9.39614075158194));
#12281=CARTESIAN_POINT('Ctrl Pts',(13.8834175105647,7.35769011342039,-10.5187877262285));
#12282=CARTESIAN_POINT('Ctrl Pts',(15.8,8.89398864851946,-11.6410274453888));
#12283=CARTESIAN_POINT('Ctrl Pts',(10.0502525316942,4.40914912230233,-8.56182484570056));
#12284=CARTESIAN_POINT('Ctrl Pts',(11.9668350211295,5.99475261978217,-9.7265265614502));
#12285=CARTESIAN_POINT('Ctrl Pts',(13.8834175105647,7.57996568930601,-10.8916014121612));
#12286=CARTESIAN_POINT('Ctrl Pts',(15.8,9.16556918678585,-12.0563031279108));
#12287=CARTESIAN_POINT('Ctrl Pts',(10.0502525316941,4.43426842278353,-9.14929101108337));
#12288=CARTESIAN_POINT('Ctrl Pts',(11.9668350211294,6.0771653528682,-10.4198746943315));
#12289=CARTESIAN_POINT('Ctrl Pts',(13.8834175105647,7.7203916302128,-11.6903432820695));
#12290=CARTESIAN_POINT('Ctrl Pts',(15.7999999999999,9.36328856029747,-12.9609269653176));
#12291=CARTESIAN_POINT('Ctrl Pts',(10.0502525316942,4.36559112518463,-9.59390955692677));
#12292=CARTESIAN_POINT('Ctrl Pts',(11.9668350211294,6.03655897381968,-10.9506581995853));
#12293=CARTESIAN_POINT('Ctrl Pts',(13.8834175105647,7.70675651927341,-12.30814436114));
#12294=CARTESIAN_POINT('Ctrl Pts',(15.8,9.37772436790846,-13.6648930037986));
#12295=CARTESIAN_POINT('Ctrl Pts',(10.0502525316942,4.29750123086779,-9.86553218952114));
#12296=CARTESIAN_POINT('Ctrl Pts',(11.9668350211294,5.98055897313701,-11.2772850923971));
#12297=CARTESIAN_POINT('Ctrl Pts',(13.8834175105647,7.66361671540623,-12.689037995273));
#12298=CARTESIAN_POINT('Ctrl Pts',(15.8,9.34667445767544,-14.1007908981489));
#12299=CARTESIAN_POINT('',(10.0502525316942,4.29750123086779,-9.86553218952114));
#12300=CARTESIAN_POINT('',(15.8,8.72583437976793,-11.4594761077026));
#12301=CARTESIAN_POINT('Ctrl Pts',(15.8,8.72583437976793,-11.4594761077026));
#12302=CARTESIAN_POINT('Ctrl Pts',(15.5456576332001,8.52985067008859,-11.3172805234003));
#12303=CARTESIAN_POINT('Ctrl Pts',(15.2905271063766,8.3328583934094,-11.1743857021214));
#12304=CARTESIAN_POINT('Ctrl Pts',(15.0353293003182,8.13531790820428,-11.0310582754415));
#12305=CARTESIAN_POINT('Ctrl Pts',(14.7778810903251,7.93603545706285,-10.8864669483781));
#12306=CARTESIAN_POINT('Ctrl Pts',(14.5203644092919,7.73619524960907,-10.7414351729092));
#12307=CARTESIAN_POINT('Ctrl Pts',(14.2635193774437,7.536317168099,-10.5962621862442));
#12308=CARTESIAN_POINT('Ctrl Pts',(14.0000858106901,7.33131185594966,-10.4473652525631));
#12309=CARTESIAN_POINT('Ctrl Pts',(13.7373587930845,7.12626688447453,-10.2983195619273));
#12310=CARTESIAN_POINT('Ctrl Pts',(13.4761368746002,6.92179020337864,-10.1494777980995));
#12311=CARTESIAN_POINT('Ctrl Pts',(13.2939626340448,6.77918967312429,-10.045676649078));
#12312=CARTESIAN_POINT('Ctrl Pts',(13.1125204081991,6.6368665464255,-9.94197532369119));
#12313=CARTESIAN_POINT('Ctrl Pts',(12.9320810503802,6.49503902755748,-9.83850230979698));
#12314=CARTESIAN_POINT('Ctrl Pts',(12.7419408648007,6.34558654067317,-9.72946635277447));
#12315=CARTESIAN_POINT('Ctrl Pts',(12.5505199208776,6.1948350500801,-9.61935521332116));
#12316=CARTESIAN_POINT('Ctrl Pts',(12.3584607499554,6.04320018913792,-9.5083731166294));
#12317=CARTESIAN_POINT('Ctrl Pts',(12.1609501300797,5.88726129158026,-9.39424088015544));
#12318=CARTESIAN_POINT('Ctrl Pts',(11.9627645378629,5.73038832458546,-9.27918728832953));
#12319=CARTESIAN_POINT('Ctrl Pts',(11.7646027855806,5.57307865663086,-9.16346774534082));
#12320=CARTESIAN_POINT('Ctrl Pts',(11.5611701848689,5.41158475328924,-9.04467021094167));
#12321=CARTESIAN_POINT('Ctrl Pts',(11.3577627091815,5.24963101923089,-8.9251706806875));
#12322=CARTESIAN_POINT('Ctrl Pts',(11.1551364296869,5.08779829683645,-8.80528327914596));
#12323=CARTESIAN_POINT('Ctrl Pts',(10.9369421951535,4.91353182422793,-8.6761848232359));
#12324=CARTESIAN_POINT('Ctrl Pts',(10.7196538081806,4.73940615822496,-8.54663632684921));
#12325=CARTESIAN_POINT('Ctrl Pts',(10.5042153409026,4.5661889859333,-8.41707738748313));
#12326=CARTESIAN_POINT('Ctrl Pts',(10.3518579060906,4.44369032369729,-8.32545369600329));
#12327=CARTESIAN_POINT('Ctrl Pts',(10.2004256671343,4.32164700273164,-8.23382587572336));
#12328=CARTESIAN_POINT('Ctrl Pts',(10.0502525316942,4.20033906466803,-8.14236230483842));
#12329=CARTESIAN_POINT('Ctrl Pts',(15.8,8.72583437976793,-11.4594761077026));
#12330=CARTESIAN_POINT('Ctrl Pts',(15.8,8.73173311854078,-11.4658448066529));
#12331=CARTESIAN_POINT('Ctrl Pts',(15.8,8.73759798728384,-11.4722392320194));
#12332=CARTESIAN_POINT('Ctrl Pts',(15.8,8.74342898604263,-11.4786593837858));
#12333=CARTESIAN_POINT('Ctrl Pts',(15.8,8.7492261070902,-11.4851052678107));
#12334=CARTESIAN_POINT('Ctrl Pts',(15.8,8.7549893339674,-11.4915768952696));
#12335=CARTESIAN_POINT('Ctrl Pts',(10.0502525316942,1.47863151154858,-9.041822881172));
#12336=CARTESIAN_POINT('Ctrl Pts',(11.9668350211294,2.57161726872464,-10.5595621004509));
#12337=CARTESIAN_POINT('Ctrl Pts',(13.8834175105647,3.66460302590071,-12.0773013197298));
#12338=CARTESIAN_POINT('Ctrl Pts',(15.8,4.75758878307678,-13.5950405390087));
#12339=CARTESIAN_POINT('Ctrl Pts',(10.0502525316942,1.5185960783211,-9.19311615914592));
#12340=CARTESIAN_POINT('Ctrl Pts',(11.9668350211294,2.63291166611866,-10.7351719126775));
#12341=CARTESIAN_POINT('Ctrl Pts',(13.8834175105647,3.74709495962167,-12.2776128949465));
#12342=CARTESIAN_POINT('Ctrl Pts',(15.8,4.86141054741923,-13.8196686484781));
#12343=CARTESIAN_POINT('Ctrl Pts',(10.0502525316942,1.54760878347554,-9.50527827631687));
#12344=CARTESIAN_POINT('Ctrl Pts',(11.9668350211294,2.69569469846983,-11.1029538596823));
#12345=CARTESIAN_POINT('Ctrl Pts',(13.8834175105647,3.84329897549065,-12.7008586295609));
#12346=CARTESIAN_POINT('Ctrl Pts',(15.8,4.99138489048493,-14.2985342129264));
#12347=CARTESIAN_POINT('Ctrl Pts',(10.0502525316941,1.3899625395975,-10.0717544060046));
#12348=CARTESIAN_POINT('Ctrl Pts',(11.9668350211294,2.55981841965666,-11.7878343688586));
#12349=CARTESIAN_POINT('Ctrl Pts',(13.8834175105647,3.73002877331941,-13.5039013178588));
#12350=CARTESIAN_POINT('Ctrl Pts',(15.7999999999999,4.89988465337857,-15.2199812807128));
#12351=CARTESIAN_POINT('Ctrl Pts',(10.0502525316942,1.18724279150055,-10.473392049036));
#12352=CARTESIAN_POINT('Ctrl Pts',(11.9668350211294,2.35716926478797,-12.2800941488934));
#12353=CARTESIAN_POINT('Ctrl Pts',(13.8834175105647,3.52613523034269,-14.0872596341291));
#12354=CARTESIAN_POINT('Ctrl Pts',(15.8,4.6960617036301,-15.8939617339865));
#12355=CARTESIAN_POINT('Ctrl Pts',(10.0502525316942,1.03854944428814,-10.7106795892491));
#12356=CARTESIAN_POINT('Ctrl Pts',(11.9668350211294,2.20297683852746,-12.5734298318033));
#12357=CARTESIAN_POINT('Ctrl Pts',(13.8834175105647,3.36740423276678,-14.4361800743576));
#12358=CARTESIAN_POINT('Ctrl Pts',(15.8,4.5318316270061,-16.2989303169119));
#12359=CARTESIAN_POINT('',(10.0502525316942,1.03854944428814,-10.7106795892491));
#12360=CARTESIAN_POINT('',(15.8,4.75758878307678,-13.5950405390087));
#12361=CARTESIAN_POINT('Ctrl Pts',(15.8,4.75758878307678,-13.5950405390087));
#12362=CARTESIAN_POINT('Ctrl Pts',(15.5456573899561,4.61513791473822,-13.3992420178035));
#12363=CARTESIAN_POINT('Ctrl Pts',(15.2905266183811,4.47194392111085,-13.2024668138655));
#12364=CARTESIAN_POINT('Ctrl Pts',(15.0353285681319,4.32836223491289,-13.0051107697458));
#12365=CARTESIAN_POINT('Ctrl Pts',(14.7778801662808,4.18351443685701,-12.8060144282783));
#12366=CARTESIAN_POINT('Ctrl Pts',(14.5203632939894,4.03827228948957,-12.6063268373508));
#12367=CARTESIAN_POINT('Ctrl Pts',(14.2635180731361,3.89303775923336,-12.4064932437269));
#12368=CARTESIAN_POINT('Ctrl Pts',(14.0000842255548,3.74407765407761,-12.2015334929889));
#12369=CARTESIAN_POINT('Ctrl Pts',(13.7373569299582,3.59512579987268,-11.9964200114428));
#12370=CARTESIAN_POINT('Ctrl Pts',(13.4761347388948,3.44665140507618,-11.7916760912323));
#12371=CARTESIAN_POINT('Ctrl Pts',(13.2939612159623,3.34310697244114,-11.6488899018511));
#12372=CARTESIAN_POINT('Ctrl Pts',(13.1125197030769,3.23979551676097,-11.5062843729551));
#12373=CARTESIAN_POINT('Ctrl Pts',(12.9320810503802,3.13688485529761,-11.3640491305165));
#12374=CARTESIAN_POINT('Ctrl Pts',(12.7419408532675,3.02844105368857,-11.2141664051166));
#12375=CARTESIAN_POINT('Ctrl Pts',(12.5505198976557,2.91909407414949,-11.0628597070359));
#12376=CARTESIAN_POINT('Ctrl Pts',(12.3584607150065,2.8091760977475,-10.9104517039517));
#12377=CARTESIAN_POINT('Ctrl Pts',(12.1609503726549,2.69613835151592,-10.7537179490172));
#12378=CARTESIAN_POINT('Ctrl Pts',(11.9627650599008,2.58249696621073,-10.5958192942301));
#12379=CARTESIAN_POINT('Ctrl Pts',(11.7646035860731,2.46864604141747,-10.4371523366742));
#12380=CARTESIAN_POINT('Ctrl Pts',(11.5611715157473,2.3517669685492,-10.2742652373587));
#12381=CARTESIAN_POINT('Ctrl Pts',(11.3577645693232,2.23466749726821,-10.110568409322));
#12382=CARTESIAN_POINT('Ctrl Pts',(11.1551388120548,2.11780296935792,-9.94654008829837));
#12383=CARTESIAN_POINT('Ctrl Pts',(10.936944253188,1.99195912572073,-9.76990860950771));
#12384=CARTESIAN_POINT('Ctrl Pts',(10.7196555410841,1.86638826421828,-9.59289262515089));
#12385=CARTESIAN_POINT('Ctrl Pts',(10.5042167520016,1.7416846628415,-9.41614744679623));
#12386=CARTESIAN_POINT('Ctrl Pts',(10.3518588411106,1.65349450791511,-9.29115358543616));
#12387=CARTESIAN_POINT('Ctrl Pts',(10.2004261307571,1.56573868767392,-9.16629650496067));
#12388=CARTESIAN_POINT('Ctrl Pts',(10.0502525316942,1.47863151154858,-9.041822881172));
#12389=CARTESIAN_POINT('Ctrl Pts',(15.8,4.75758878307678,-13.5950405390087));
#12390=CARTESIAN_POINT('Ctrl Pts',(15.8,4.76123078081695,-13.6029203421718));
#12391=CARTESIAN_POINT('Ctrl Pts',(15.8,4.76483261634472,-13.610814146196));
#12392=CARTESIAN_POINT('Ctrl Pts',(15.8,4.7683942897085,-13.6187219510797));
#12393=CARTESIAN_POINT('Ctrl Pts',(15.8,4.77191579174907,-13.626643760007));
#12394=CARTESIAN_POINT('Ctrl Pts',(15.8,4.77539710335945,-13.6345795785203));
#12395=CARTESIAN_POINT('Ctrl Pts',(10.0502525316942,-1.38781479615277,-9.05620683581208));
#12396=CARTESIAN_POINT('Ctrl Pts',(11.9668350211294,-0.817330781359224,
-10.8374137839212));
#12397=CARTESIAN_POINT('Ctrl Pts',(13.8834175105647,-0.246846766565677,
-12.6186207320302));
#12398=CARTESIAN_POINT('Ctrl Pts',(15.8,0.32363724822787,-14.3998276801393));
#12399=CARTESIAN_POINT('Ctrl Pts',(10.0502525316942,-1.39655842853148,-9.21244502400637));
#12400=CARTESIAN_POINT('Ctrl Pts',(11.9668350211294,-0.813302761662288,
-11.0233696506194));
#12401=CARTESIAN_POINT('Ctrl Pts',(13.8834175105647,-0.230291956370554,
-12.8346197703481));
#12402=CARTESIAN_POINT('Ctrl Pts',(15.8,0.352963710498643,-14.6455443969611));
#12403=CARTESIAN_POINT('Ctrl Pts',(10.0502525316942,-1.46541714813614,-9.51829373400973));
#12404=CARTESIAN_POINT('Ctrl Pts',(11.9668350211295,-0.867231464171971,
-11.3925515672309));
#12405=CARTESIAN_POINT('Ctrl Pts',(13.8834175105647,-0.269566015193986,
-13.2668740653714));
#12406=CARTESIAN_POINT('Ctrl Pts',(15.8,0.328619668770179,-15.1411318985925));
#12407=CARTESIAN_POINT('Ctrl Pts',(10.0502525316941,-1.7903975044951,-10.0083300006652));
#12408=CARTESIAN_POINT('Ctrl Pts',(11.9668350211294,-1.20809631886685,-12.0019243797287));
#12409=CARTESIAN_POINT('Ctrl Pts',(13.8834175105647,-0.625444427693872,
-13.9956114385883));
#12410=CARTESIAN_POINT('Ctrl Pts',(15.8,-0.0431432420656229,-15.9892058176518));
#12411=CARTESIAN_POINT('Ctrl Pts',(10.0502525316942,-2.10732113862255,-10.3276659549724));
#12412=CARTESIAN_POINT('Ctrl Pts',(11.9668350211294,-1.55295659524519,-12.4074689224609));
#12413=CARTESIAN_POINT('Ctrl Pts',(13.8834175105647,-0.999648742962751,
-14.4874157824203));
#12414=CARTESIAN_POINT('Ctrl Pts',(15.8,-0.445284199585383,-16.5672187499088));
#12415=CARTESIAN_POINT('Ctrl Pts',(10.0502525316942,-2.32206279789789,-10.5073910450885));
#12416=CARTESIAN_POINT('Ctrl Pts',(11.9668350211294,-1.79024801807933,-12.6387996550358));
#12417=CARTESIAN_POINT('Ctrl Pts',(13.8834175105647,-1.25843323826077,-14.7702082649831));
#12418=CARTESIAN_POINT('Ctrl Pts',(15.8,-0.726618458442201,-16.9016168749304));
#12419=CARTESIAN_POINT('',(10.0502525316942,-2.32206279789789,-10.5073910450885));
#12420=CARTESIAN_POINT('',(15.8,0.32363724822787,-14.3998276801393));
#12421=CARTESIAN_POINT('Ctrl Pts',(15.8,0.32363724822787,-14.3998276801393));
#12422=CARTESIAN_POINT('Ctrl Pts',(15.5456570571815,0.248663394074979,-14.169592180253));
#12423=CARTESIAN_POINT('Ctrl Pts',(15.2905259507696,0.173284602939125,-13.938198156862));
#12424=CARTESIAN_POINT('Ctrl Pts',(15.0353275664506,0.0977165877036246,
-13.7061319160824));
#12425=CARTESIAN_POINT('Ctrl Pts',(14.7778789011639,0.0214822309985085,
-13.4720193682845));
#12426=CARTESIAN_POINT('Ctrl Pts',(14.5203617662566,-0.0549444640653608,
-13.2372226466649));
#12427=CARTESIAN_POINT('Ctrl Pts',(14.2635162858779,-0.131318796806587,
-13.002289423513));
#12428=CARTESIAN_POINT('Ctrl Pts',(14.0000820510449,-0.209652329780965,
-12.7613295522838));
#12429=CARTESIAN_POINT('Ctrl Pts',(13.7373543720969,-0.287930509547997,
-12.5202260255142));
#12430=CARTESIAN_POINT('Ctrl Pts',(13.4761318051332,-0.365868800888249,
-12.2796215208027));
#12431=CARTESIAN_POINT('Ctrl Pts',(13.2939592679802,-0.420221747648761,
-12.111827698151));
#12432=CARTESIAN_POINT('Ctrl Pts',(13.1125187344693,-0.47440895039499,-11.9442776868938));
#12433=CARTESIAN_POINT('Ctrl Pts',(12.9320810503802,-0.528329405335827,
-11.7772036867065));
#12434=CARTESIAN_POINT('Ctrl Pts',(12.7419408368629,-0.585149281223488,
-11.6011457516407));
#12435=CARTESIAN_POINT('Ctrl Pts',(12.5505198646257,-0.642388101081619,
-11.4234544410905));
#12436=CARTESIAN_POINT('Ctrl Pts',(12.3584606652962,-0.699829652728586,
-11.2445392798278));
#12437=CARTESIAN_POINT('Ctrl Pts',(12.1609507027341,-0.758901432445018,
-11.0605463915612));
#12438=CARTESIAN_POINT('Ctrl Pts',(11.9627657724245,-0.818187336021259,
-10.8752590885153));
#12439=CARTESIAN_POINT('Ctrl Pts',(11.7646046796641,-0.877435109078444,
-10.6891763370114));
#12440=CARTESIAN_POINT('Ctrl Pts',(11.5611733353989,-0.938258623673827,
-10.4981445670725));
#12441=CARTESIAN_POINT('Ctrl Pts',(11.3577671135011,-0.999041534289407,
-10.3062745975164));
#12442=CARTESIAN_POINT('Ctrl Pts',(11.1551420711286,-1.05949856916791,-10.1141619588668));
#12443=CARTESIAN_POINT('Ctrl Pts',(10.9369470578857,-1.12460120096249,-9.90728713607363));
#12444=CARTESIAN_POINT('Ctrl Pts',(10.719657890403,-1.1893253951373,-9.70013097729617));
#12445=CARTESIAN_POINT('Ctrl Pts',(10.50421865072,-1.25330845309604,-9.49350036754002));
#12446=CARTESIAN_POINT('Ctrl Pts',(10.3518600992362,-1.2985572482758,-9.34737127591778));
#12447=CARTESIAN_POINT('Ctrl Pts',(10.2004267545894,-1.34343522942956,-9.201506488161));
#12448=CARTESIAN_POINT('Ctrl Pts',(10.0502525316942,-1.38781479615277,-9.05620683581208));
#12449=CARTESIAN_POINT('Ctrl Pts',(15.8,0.32363724822787,-14.3998276801393));
#12450=CARTESIAN_POINT('Ctrl Pts',(15.8,0.324666000821257,-14.4084472574799));
#12451=CARTESIAN_POINT('Ctrl Pts',(15.8,0.325652230376828,-14.4170677396245));
#12452=CARTESIAN_POINT('Ctrl Pts',(15.8,0.326595936941116,-14.4256891265865));
#12453=CARTESIAN_POINT('Ctrl Pts',(15.8,0.327497110819208,-14.434311418564));
#12454=CARTESIAN_POINT('Ctrl Pts',(15.8,0.328355732126618,-14.4429346149236));
#12455=CARTESIAN_POINT('Ctrl Pts',(10.0502525316942,-4.11841212213242,-8.18410616705958));
#12456=CARTESIAN_POINT('Ctrl Pts',(11.9668350211294,-4.12627279988524,-10.0544238975194));
#12457=CARTESIAN_POINT('Ctrl Pts',(13.8834175105647,-4.13413347763806,-11.9247416279792));
#12458=CARTESIAN_POINT('Ctrl Pts',(15.8,-4.14199415539088,-13.795059358439));
#12459=CARTESIAN_POINT('Ctrl Pts',(10.0502525316942,-4.17500806600467,-8.32999558303832));
#12460=CARTESIAN_POINT('Ctrl Pts',(11.9668350211294,-4.17990544851818,-10.2325231628261));
#12461=CARTESIAN_POINT('Ctrl Pts',(13.8834175105647,-4.18513629113482,-12.1352846385738));
#12462=CARTESIAN_POINT('Ctrl Pts',(15.8,-4.19003367364834,-14.0378122183616));
#12463=CARTESIAN_POINT('Ctrl Pts',(10.0502525316942,-4.33502367302149,-8.59959242261694));
#12464=CARTESIAN_POINT('Ctrl Pts',(11.9668350211295,-4.34529280263859,-10.5669670902559));
#12465=CARTESIAN_POINT('Ctrl Pts',(13.8834175105647,-4.3560888733651,-12.5342444956751));
#12466=CARTESIAN_POINT('Ctrl Pts',(15.8,-4.36635800298221,-14.5016191633141));
#12467=CARTESIAN_POINT('Ctrl Pts',(10.0502525316941,-4.79552866926091,-8.9652188127798));
#12468=CARTESIAN_POINT('Ctrl Pts',(11.9668350211294,-4.85778187524378,-11.0411807000414));
#12469=CARTESIAN_POINT('Ctrl Pts',(13.8834175105647,-4.91974349130655,-13.1173407686982));
#12470=CARTESIAN_POINT('Ctrl Pts',(15.8,-4.98199669728942,-15.1933026559598));
#12471=CARTESIAN_POINT('Ctrl Pts',(10.0502525316942,-5.19560579312754,-9.17099596015618));
#12472=CARTESIAN_POINT('Ctrl Pts',(11.9668350211294,-5.3110682436509,-11.3203141899786));
#12473=CARTESIAN_POINT('Ctrl Pts',(13.8834175105647,-5.42758013234469,-13.4694427341669));
#12474=CARTESIAN_POINT('Ctrl Pts',(15.8,-5.54304258286804,-15.6187609639894));
#12475=CARTESIAN_POINT('Ctrl Pts',(10.0502525316942,-5.45537535466284,-9.2755658561365));
#12476=CARTESIAN_POINT('Ctrl Pts',(11.9668350211294,-5.60823092528512,-11.4669957083382));
#12477=CARTESIAN_POINT('Ctrl Pts',(13.8834175105647,-5.76108649590741,-13.6584255605399));
#12478=CARTESIAN_POINT('Ctrl Pts',(15.8,-5.91394206652969,-15.8498554127416));
#12479=CARTESIAN_POINT('',(10.0502525316942,-5.45537535466284,-9.2755658561365));
#12480=CARTESIAN_POINT('',(15.8,-4.14199415539088,-13.795059358439));
#12481=CARTESIAN_POINT('Ctrl Pts',(15.8,-4.14199415539088,-13.795059358439));
#12482=CARTESIAN_POINT('Ctrl Pts',(15.5456574794166,-4.14215184549968,-13.5529245928915));
#12483=CARTESIAN_POINT('Ctrl Pts',(15.2905267978566,-4.14233665870497,-13.3095628770613));
#12484=CARTESIAN_POINT('Ctrl Pts',(15.0353288374161,-4.14249371366664,-13.0655033718487));
#12485=CARTESIAN_POINT('Ctrl Pts',(14.7778805061951,-4.1426521535606,-12.8192917162886));
#12486=CARTESIAN_POINT('Ctrl Pts',(14.5203637043132,-4.14278210218064,-12.5723699372164));
#12487=CARTESIAN_POINT('Ctrl Pts',(14.2635185530402,-4.14282007025482,-12.3253345162743));
#12488=CARTESIAN_POINT('Ctrl Pts',(14.0000848089565,-4.14285901228618,-12.0719621417617));
#12489=CARTESIAN_POINT('Ctrl Pts',(13.7373576158128,-4.14280091850188,-11.818470245772));
#12490=CARTESIAN_POINT('Ctrl Pts',(13.4761355252086,-4.14257377376942,-11.565557973583));
#12491=CARTESIAN_POINT('Ctrl Pts',(13.2939617380651,-4.14241536520587,-11.3891793743108));
#12492=CARTESIAN_POINT('Ctrl Pts',(13.1125199626854,-4.14217466317553,-11.2130838733124));
#12493=CARTESIAN_POINT('Ctrl Pts',(12.9320810503802,-4.14182735974364,-11.0375235228707));
#12494=CARTESIAN_POINT('Ctrl Pts',(12.7419408575527,-4.14146138357661,-10.8525241873096));
#12495=CARTESIAN_POINT('Ctrl Pts',(12.5505199062839,-4.14098910290385,-10.6658419590986));
#12496=CARTESIAN_POINT('Ctrl Pts',(12.3584607279919,-4.14033143664814,-10.4779331330928));
#12497=CARTESIAN_POINT('Ctrl Pts',(12.1609502835647,-4.13965510367823,-10.2846908414917));
#12498=CARTESIAN_POINT('Ctrl Pts',(11.9627648680217,-4.13878241284077,-10.0901513147856));
#12499=CARTESIAN_POINT('Ctrl Pts',(11.7646032917758,-4.13762764472381,-9.89486705365855));
#12500=CARTESIAN_POINT('Ctrl Pts',(11.5611710263533,-4.13644216215691,-9.69438863400203));
#12501=CARTESIAN_POINT('Ctrl Pts',(11.3577638852452,-4.13495903745938,-9.49312558221419));
#12502=CARTESIAN_POINT('Ctrl Pts',(11.155137935881,-4.13309099161788,-9.29173244420118));
#12503=CARTESIAN_POINT('Ctrl Pts',(10.9369434970446,-4.13107941701263,-9.07486553810084));
#12504=CARTESIAN_POINT('Ctrl Pts',(10.7196549052583,-4.12862098831911,-8.85784801697248));
#12505=CARTESIAN_POINT('Ctrl Pts',(10.5042162352539,-4.12562010893632,-8.64155934493092));
#12506=CARTESIAN_POINT('Ctrl Pts',(10.3518584987042,-4.12349789387431,-8.48860048887722));
#12507=CARTESIAN_POINT('Ctrl Pts',(10.2004259609774,-4.12110469363328,-8.33600758581804));
#12508=CARTESIAN_POINT('Ctrl Pts',(10.0502525316942,-4.11841212213242,-8.18410616705958));
#12509=CARTESIAN_POINT('Ctrl Pts',(15.8,-4.14199415539088,-13.795059358439));
#12510=CARTESIAN_POINT('Ctrl Pts',(15.8,-4.14367934941586,-13.8035749656708));
#12511=CARTESIAN_POINT('Ctrl Pts',(15.8,-4.14540526485286,-13.8120782930811));
#12512=CARTESIAN_POINT('Ctrl Pts',(15.8,-4.14717190166177,-13.8205693406969));
#12513=CARTESIAN_POINT('Ctrl Pts',(15.8,-4.14897926912419,-13.8290481057107));
#12514=CARTESIAN_POINT('Ctrl Pts',(15.8,-4.15082738595568,-13.8375145813754));
#12515=CARTESIAN_POINT('Ctrl Pts',(10.0502525316942,-6.44587057493322,-6.51088816465466));
#12516=CARTESIAN_POINT('Ctrl Pts',(11.9668350211294,-7.03130648732539,-8.28723694673789));
#12517=CARTESIAN_POINT('Ctrl Pts',(13.8834175105647,-7.61674239971757,-10.0635857288211));
#12518=CARTESIAN_POINT('Ctrl Pts',(15.8,-8.20217831210975,-11.8399345109044));
#12519=CARTESIAN_POINT('Ctrl Pts',(10.0502525316942,-6.54477882498566,-6.63214813591052));
#12520=CARTESIAN_POINT('Ctrl Pts',(11.9668350211294,-7.13734986695939,-8.4400460136743));
#12521=CARTESIAN_POINT('Ctrl Pts',(13.8834175105647,-7.73031032616364,-10.2480632948761));
#12522=CARTESIAN_POINT('Ctrl Pts',(15.8,-8.32288136813736,-12.0559611726399));
#12523=CARTESIAN_POINT('Ctrl Pts',(10.0502525316942,-6.78027814405441,-6.83909882511009));
#12524=CARTESIAN_POINT('Ctrl Pts',(11.9668350211295,-7.39799687329663,-8.70700998719297));
#12525=CARTESIAN_POINT('Ctrl Pts',(13.8834175105647,-8.01619193743949,-10.5746650104356));
#12526=CARTESIAN_POINT('Ctrl Pts',(15.8,-8.6339106666817,-12.4425761725185));
#12527=CARTESIAN_POINT('Ctrl Pts',(10.0502525316941,-7.33122941665115,-7.04452561799895));
#12528=CARTESIAN_POINT('Ctrl Pts',(11.9668350211294,-8.03194323669995,-8.99964539985646));
#12529=CARTESIAN_POINT('Ctrl Pts',(13.8834175105647,-8.73244671395173,-10.9550426722922));
#12530=CARTESIAN_POINT('Ctrl Pts',(15.8,-9.43316053400054,-12.9101624541497));
#12531=CARTESIAN_POINT('Ctrl Pts',(10.0502525316942,-7.77530835268703,-7.11660498267375));
#12532=CARTESIAN_POINT('Ctrl Pts',(11.9668350211294,-8.54929552797968,-9.12504823131445));
#12533=CARTESIAN_POINT('Ctrl Pts',(13.8834175105647,-9.32422216219831,-11.1329867839675));
#12534=CARTESIAN_POINT('Ctrl Pts',(15.8,-10.098209337491,-13.1414300326082));
#12535=CARTESIAN_POINT('Ctrl Pts',(10.0502525316942,-8.05467776187827,-7.13578365451838));
#12536=CARTESIAN_POINT('Ctrl Pts',(11.9668350211294,-8.8772411146815,-9.17272232645135));
#12537=CARTESIAN_POINT('Ctrl Pts',(13.8834175105647,-9.69980446748474,-11.2096609983843));
#12538=CARTESIAN_POINT('Ctrl Pts',(15.8,-10.522367820288,-13.2465996703173));
#12539=CARTESIAN_POINT('',(10.0502525316942,-8.05467776187827,-7.13578365451838));
#12540=CARTESIAN_POINT('',(15.8,-8.20217831210975,-11.8399345109044));
#12541=CARTESIAN_POINT('Ctrl Pts',(15.8,-8.20217831210975,-11.8399345109044));
#12542=CARTESIAN_POINT('Ctrl Pts',(15.5456576615063,-8.12750458029281,-11.6096021002858));
#12543=CARTESIAN_POINT('Ctrl Pts',(15.2905271631646,-8.05247749955168,-11.3780944093842));
#12544=CARTESIAN_POINT('Ctrl Pts',(15.0353293855227,-7.97720839274395,-11.1459316587082));
#12545=CARTESIAN_POINT('Ctrl Pts',(14.7778811978172,-7.90127554051884,-10.9117216277018));
#12546=CARTESIAN_POINT('Ctrl Pts',(14.5203645390018,-7.82509615349566,-10.6768450327834));
#12547=CARTESIAN_POINT('Ctrl Pts',(14.2635195291096,-7.74879417034655,-10.4418887807018));
#12548=CARTESIAN_POINT('Ctrl Pts',(14.0000859949164,-7.6705349077066,-10.2009054892895));
#12549=CARTESIAN_POINT('Ctrl Pts',(13.7373590095418,-7.59214642417304,-9.95983851105689));
#12550=CARTESIAN_POINT('Ctrl Pts',(13.4761371226606,-7.51377627479466,-9.71937502566798));
#12551=CARTESIAN_POINT('Ctrl Pts',(13.2939627987539,-7.45912147864444,-9.55167746633259));
#12552=CARTESIAN_POINT('Ctrl Pts',(13.1125204900985,-7.40447589782759,-9.38427458086197));
#12553=CARTESIAN_POINT('Ctrl Pts',(12.9320810503802,-7.34989430276011,-9.21741359915303));
#12554=CARTESIAN_POINT('Ctrl Pts',(12.7419408661185,-7.29237830426427,-9.04158187490387));
#12555=CARTESIAN_POINT('Ctrl Pts',(12.550519923531,-7.23424116054673,-8.86418247516815));
#12556=CARTESIAN_POINT('Ctrl Pts',(12.3584607539488,-7.17554866346933,-8.68567379986729));
#12557=CARTESIAN_POINT('Ctrl Pts',(12.1609501017824,-7.11519021560012,-8.50209826451157));
#12558=CARTESIAN_POINT('Ctrl Pts',(11.9627644770494,-7.0542441495791,-8.31734966162915));
#12559=CARTESIAN_POINT('Ctrl Pts',(11.7646026923681,-6.99279967398827,-8.13197994128727));
#12560=CARTESIAN_POINT('Ctrl Pts',(11.5611700299535,-6.92972084534216,-7.9416795975511));
#12561=CARTESIAN_POINT('Ctrl Pts',(11.3577624926939,-6.8661164739041,-7.7507250000513));
#12562=CARTESIAN_POINT('Ctrl Pts',(11.1551361524457,-6.80210582000323,-7.55976563308483));
#12563=CARTESIAN_POINT('Ctrl Pts',(10.9369419552413,-6.73317720379604,-7.35413478705123));
#12564=CARTESIAN_POINT('Ctrl Pts',(10.7196536056938,-6.66377706212423,-7.14849878641362));
#12565=CARTESIAN_POINT('Ctrl Pts',(10.5042151754627,-6.59408624907933,-6.94372358733722));
#12566=CARTESIAN_POINT('Ctrl Pts',(10.3518577964671,-6.54480112569535,-6.79890721181355));
#12567=CARTESIAN_POINT('Ctrl Pts',(10.2004256127783,-6.49537136769562,-6.65452261540872));
#12568=CARTESIAN_POINT('Ctrl Pts',(10.0502525316942,-6.44587057493322,-6.51088816465466));
#12569=CARTESIAN_POINT('Ctrl Pts',(15.8,-8.20217831210975,-11.8399345109044));
#12570=CARTESIAN_POINT('Ctrl Pts',(15.8,-8.20641249422049,-11.8475125810599));
#12571=CARTESIAN_POINT('Ctrl Pts',(15.8,-8.21068161002192,-11.8550663888027));
#12572=CARTESIAN_POINT('Ctrl Pts',(15.8,-8.21498565948429,-11.862595934171));
#12573=CARTESIAN_POINT('Ctrl Pts',(15.8,-8.21932465056734,-11.8701012116266));
#12574=CARTESIAN_POINT('Ctrl Pts',(15.8,-8.22369859898568,-11.8775822089691));
#12575=CARTESIAN_POINT('Ctrl Pts',(10.0502525316942,-8.14236230483842,-4.20033906466803));
#12576=CARTESIAN_POINT('Ctrl Pts',(11.9668350211294,-9.24806690579316,-5.70883750303466));
#12577=CARTESIAN_POINT('Ctrl Pts',(13.8834175105647,-10.3537715067479,-7.21733594140129));
#12578=CARTESIAN_POINT('Ctrl Pts',(15.8,-11.4594761077026,-8.72583437976793));
#12579=CARTESIAN_POINT('Ctrl Pts',(10.0502525316942,-8.27390103242161,-4.28509982034658));
#12580=CARTESIAN_POINT('Ctrl Pts',(11.9668350211294,-9.39614075158194,-5.82139835544565));
#12581=CARTESIAN_POINT('Ctrl Pts',(13.8834175105647,-10.5187877262285,-7.35769011342039));
#12582=CARTESIAN_POINT('Ctrl Pts',(15.8,-11.6410274453888,-8.89398864851946));
#12583=CARTESIAN_POINT('Ctrl Pts',(10.0502525316942,-8.56182484570057,-4.40914912230233));
#12584=CARTESIAN_POINT('Ctrl Pts',(11.9668350211295,-9.72652656145021,-5.99475261978216));
#12585=CARTESIAN_POINT('Ctrl Pts',(13.8834175105647,-10.8916014121611,-7.57996568930606));
#12586=CARTESIAN_POINT('Ctrl Pts',(15.8,-12.0563031279108,-9.1655691867859));
#12587=CARTESIAN_POINT('Ctrl Pts',(10.0502525316941,-9.14929101108337,-4.43426842278354));
#12588=CARTESIAN_POINT('Ctrl Pts',(11.9668350211294,-10.4198746943315,-6.07716535286821));
#12589=CARTESIAN_POINT('Ctrl Pts',(13.8834175105647,-11.6903432820695,-7.72039163021283));
#12590=CARTESIAN_POINT('Ctrl Pts',(15.7999999999999,-12.9609269653176,-9.36328856029751));
#12591=CARTESIAN_POINT('Ctrl Pts',(10.0502525316942,-9.59390955692679,-4.36559112518464));
#12592=CARTESIAN_POINT('Ctrl Pts',(11.9668350211294,-10.9506581995854,-6.03655897381969));
#12593=CARTESIAN_POINT('Ctrl Pts',(13.8834175105647,-12.30814436114,-7.70675651927339));
#12594=CARTESIAN_POINT('Ctrl Pts',(15.8,-13.6648930037986,-9.37772436790844));
#12595=CARTESIAN_POINT('Ctrl Pts',(10.0502525316942,-9.86553218952113,-4.29750123086779));
#12596=CARTESIAN_POINT('Ctrl Pts',(11.9668350211294,-11.2772850923971,-5.98055897313701));
#12597=CARTESIAN_POINT('Ctrl Pts',(13.8834175105647,-12.689037995273,-7.66361671540623));
#12598=CARTESIAN_POINT('Ctrl Pts',(15.8,-14.1007908981489,-9.34667445767544));
#12599=CARTESIAN_POINT('',(10.0502525316942,-9.86553218952113,-4.29750123086779));
#12600=CARTESIAN_POINT('',(15.8,-11.4594761077026,-8.72583437976793));
#12601=CARTESIAN_POINT('Ctrl Pts',(15.8,-11.4594761077026,-8.72583437976793));
#12602=CARTESIAN_POINT('Ctrl Pts',(15.5456576332011,-11.3172805234009,-8.52985067008938));
#12603=CARTESIAN_POINT('Ctrl Pts',(15.2905271063787,-11.1743857021226,-8.33285839341101));
#12604=CARTESIAN_POINT('Ctrl Pts',(15.0353293003213,-11.0310582754433,-8.13531790820672));
#12605=CARTESIAN_POINT('Ctrl Pts',(14.777881090327,-10.8864669483792,-7.93603545706437));
#12606=CARTESIAN_POINT('Ctrl Pts',(14.5203644092926,-10.7414351729097,-7.73619524960966));
#12607=CARTESIAN_POINT('Ctrl Pts',(14.2635193774432,-10.596262186244,-7.53631716809867));
#12608=CARTESIAN_POINT('Ctrl Pts',(14.000085810689,-10.4473652525625,-7.33131185594875));
#12609=CARTESIAN_POINT('Ctrl Pts',(13.7373587930826,-10.2983195619262,-7.12626688447304));
#12610=CARTESIAN_POINT('Ctrl Pts',(13.4761368745975,-10.149477798098,-6.92179020337659));
#12611=CARTESIAN_POINT('Ctrl Pts',(13.293962634043,-10.0456766490771,-6.77918967312293));
#12612=CARTESIAN_POINT('Ctrl Pts',(13.1125204081982,-9.94197532369069,-6.63686654642483));
#12613=CARTESIAN_POINT('Ctrl Pts',(12.9320810503802,-9.83850230979698,-6.49503902755748));
#12614=CARTESIAN_POINT('Ctrl Pts',(12.7419408648011,-9.72946635277469,-6.34558654067346));
#12615=CARTESIAN_POINT('Ctrl Pts',(12.5505199208783,-9.61935521332159,-6.19483505008069));
#12616=CARTESIAN_POINT('Ctrl Pts',(12.3584607499565,-9.50837311663005,-6.0432001891388));
#12617=CARTESIAN_POINT('Ctrl Pts',(12.1609501300809,-9.39424088015611,-5.88726129158117));
#12618=CARTESIAN_POINT('Ctrl Pts',(11.9627645378641,-9.27918728833022,-5.73038832458639));
#12619=CARTESIAN_POINT('Ctrl Pts',(11.7646027855818,-9.16346774534153,-5.57307865663182));
#12620=CARTESIAN_POINT('Ctrl Pts',(11.56117018487,-9.0446702109423,-5.41158475329009));
#12621=CARTESIAN_POINT('Ctrl Pts',(11.3577627091825,-8.92517068068805,-5.24963101923163));
#12622=CARTESIAN_POINT('Ctrl Pts',(11.1551364296877,-8.80528327914643,-5.08779829683707));
#12623=CARTESIAN_POINT('Ctrl Pts',(10.9369421951543,-8.67618482323638,-4.91353182422858));
#12624=CARTESIAN_POINT('Ctrl Pts',(10.7196538081815,-8.54663632684971,-4.73940615822563));
#12625=CARTESIAN_POINT('Ctrl Pts',(10.5042153409034,-8.41707738748364,-4.56618898593399));
#12626=CARTESIAN_POINT('Ctrl Pts',(10.3518579060912,-8.32545369600363,-4.44369032369775));
#12627=CARTESIAN_POINT('Ctrl Pts',(10.2004256671345,-8.23382587572353,-4.32164700273186));
#12628=CARTESIAN_POINT('Ctrl Pts',(10.0502525316942,-8.14236230483842,-4.20033906466803));
#12629=CARTESIAN_POINT('Ctrl Pts',(15.8,-11.4594761077026,-8.72583437976793));
#12630=CARTESIAN_POINT('Ctrl Pts',(15.8,-11.4658448066529,-8.73173311854078));
#12631=CARTESIAN_POINT('Ctrl Pts',(15.8,-11.4722392320194,-8.73759798728384));
#12632=CARTESIAN_POINT('Ctrl Pts',(15.8,-11.4786593837858,-8.74342898604263));
#12633=CARTESIAN_POINT('Ctrl Pts',(15.8,-11.4851052678107,-8.74922610709021));
#12634=CARTESIAN_POINT('Ctrl Pts',(15.8,-11.4915768952696,-8.7549893339674));
#12635=CARTESIAN_POINT('Ctrl Pts',(10.0502525316942,-9.041822881172,-1.47863151154858));
#12636=CARTESIAN_POINT('Ctrl Pts',(11.9668350211294,-10.5595621004509,-2.57161726872464));
#12637=CARTESIAN_POINT('Ctrl Pts',(13.8834175105647,-12.0773013197298,-3.66460302590071));
#12638=CARTESIAN_POINT('Ctrl Pts',(15.8,-13.5950405390087,-4.75758878307678));
#12639=CARTESIAN_POINT('Ctrl Pts',(10.0502525316942,-9.19311615914592,-1.5185960783211));
#12640=CARTESIAN_POINT('Ctrl Pts',(11.9668350211294,-10.7351719126775,-2.63291166611866));
#12641=CARTESIAN_POINT('Ctrl Pts',(13.8834175105647,-12.2776128949465,-3.74709495962168));
#12642=CARTESIAN_POINT('Ctrl Pts',(15.8,-13.8196686484781,-4.86141054741924));
#12643=CARTESIAN_POINT('Ctrl Pts',(10.0502525316942,-9.50527827631687,-1.54760878347554));
#12644=CARTESIAN_POINT('Ctrl Pts',(11.9668350211294,-11.1029538596823,-2.69569469846983));
#12645=CARTESIAN_POINT('Ctrl Pts',(13.8834175105647,-12.7008586295609,-3.84329897549064));
#12646=CARTESIAN_POINT('Ctrl Pts',(15.8,-14.2985342129264,-4.99138489048493));
#12647=CARTESIAN_POINT('Ctrl Pts',(10.0502525316941,-10.0717544060046,-1.38996253959751));
#12648=CARTESIAN_POINT('Ctrl Pts',(11.9668350211294,-11.7878343688586,-2.55981841965666));
#12649=CARTESIAN_POINT('Ctrl Pts',(13.8834175105647,-13.5039013178588,-3.73002877331942));
#12650=CARTESIAN_POINT('Ctrl Pts',(15.7999999999999,-15.2199812807128,-4.89988465337858));
#12651=CARTESIAN_POINT('Ctrl Pts',(10.0502525316942,-10.473392049036,-1.18724279150055));
#12652=CARTESIAN_POINT('Ctrl Pts',(11.9668350211294,-12.2800941488934,-2.35716926478797));
#12653=CARTESIAN_POINT('Ctrl Pts',(13.8834175105647,-14.0872596341291,-3.52613523034269));
#12654=CARTESIAN_POINT('Ctrl Pts',(15.8,-15.8939617339865,-4.6960617036301));
#12655=CARTESIAN_POINT('Ctrl Pts',(10.0502525316942,-10.7106795892491,-1.03854944428814));
#12656=CARTESIAN_POINT('Ctrl Pts',(11.9668350211294,-12.5734298318033,-2.20297683852746));
#12657=CARTESIAN_POINT('Ctrl Pts',(13.8834175105647,-14.4361800743576,-3.36740423276678));
#12658=CARTESIAN_POINT('Ctrl Pts',(15.8,-16.2989303169119,-4.5318316270061));
#12659=CARTESIAN_POINT('',(10.0502525316942,-10.7106795892491,-1.03854944428814));
#12660=CARTESIAN_POINT('',(15.8,-13.5950405390087,-4.75758878307678));
#12661=CARTESIAN_POINT('Ctrl Pts',(15.8,-13.5950405390087,-4.75758878307678));
#12662=CARTESIAN_POINT('Ctrl Pts',(15.5456573899571,-13.3992420178043,-4.61513791473879));
#12663=CARTESIAN_POINT('Ctrl Pts',(15.2905266183831,-13.202466813867,-4.47194392111198));
#12664=CARTESIAN_POINT('Ctrl Pts',(15.0353285681349,-13.0051107697481,-4.32836223491455));
#12665=CARTESIAN_POINT('Ctrl Pts',(14.7778801662826,-12.8060144282797,-4.18351443685803));
#12666=CARTESIAN_POINT('Ctrl Pts',(14.52036329399,-12.6063268373513,-4.03827228948993));
#12667=CARTESIAN_POINT('Ctrl Pts',(14.2635180731355,-12.4064932437265,-3.89303775923306));
#12668=CARTESIAN_POINT('Ctrl Pts',(14.0000842255552,-12.2015334929893,-3.74407765407785));
#12669=CARTESIAN_POINT('Ctrl Pts',(13.7373569299596,-11.9964200114439,-3.59512579987346));
#12670=CARTESIAN_POINT('Ctrl Pts',(13.4761347388971,-11.7916760912341,-3.44665140507749));
#12671=CARTESIAN_POINT('Ctrl Pts',(13.2939612159639,-11.6488899018523,-3.34310697244201));
#12672=CARTESIAN_POINT('Ctrl Pts',(13.1125197030777,-11.5062843729557,-3.2397955167614));
#12673=CARTESIAN_POINT('Ctrl Pts',(12.9320810503802,-11.3640491305165,-3.13688485529761));
#12674=CARTESIAN_POINT('Ctrl Pts',(12.7419408532673,-11.2141664051165,-3.02844105368848));
#12675=CARTESIAN_POINT('Ctrl Pts',(12.5505198976554,-11.0628597070356,-2.91909407414931));
#12676=CARTESIAN_POINT('Ctrl Pts',(12.358460715006,-10.9104517039513,-2.80917609774724));
#12677=CARTESIAN_POINT('Ctrl Pts',(12.1609503726544,-10.7537179490168,-2.69613835151564));
#12678=CARTESIAN_POINT('Ctrl Pts',(11.9627650599002,-10.5958192942297,-2.58249696621042));
#12679=CARTESIAN_POINT('Ctrl Pts',(11.7646035860725,-10.4371523366737,-2.46864604141714));
#12680=CARTESIAN_POINT('Ctrl Pts',(11.5611715157468,-10.2742652373582,-2.35176696854891));
#12681=CARTESIAN_POINT('Ctrl Pts',(11.3577645693228,-10.1105684093216,-2.23466749726794));
#12682=CARTESIAN_POINT('Ctrl Pts',(11.1551388120544,-9.94654008829804,-2.11780296935768));
#12683=CARTESIAN_POINT('Ctrl Pts',(10.9369442531875,-9.7699086095073,-1.99195912572045));
#12684=CARTESIAN_POINT('Ctrl Pts',(10.7196555410835,-9.59289262515041,-1.86638826421794));
#12685=CARTESIAN_POINT('Ctrl Pts',(10.5042167520009,-9.41614744679567,-1.74168466284111));
#12686=CARTESIAN_POINT('Ctrl Pts',(10.3518588411102,-9.29115358543579,-1.65349450791485));
#12687=CARTESIAN_POINT('Ctrl Pts',(10.2004261307569,-9.16629650496048,-1.56573868767379));
#12688=CARTESIAN_POINT('Ctrl Pts',(10.0502525316942,-9.041822881172,-1.47863151154858));
#12689=CARTESIAN_POINT('Ctrl Pts',(15.8,-13.5950405390087,-4.75758878307678));
#12690=CARTESIAN_POINT('Ctrl Pts',(15.8,-13.6029203421718,-4.76123078081695));
#12691=CARTESIAN_POINT('Ctrl Pts',(15.8,-13.610814146196,-4.76483261634472));
#12692=CARTESIAN_POINT('Ctrl Pts',(15.8,-13.6187219510797,-4.7683942897085));
#12693=CARTESIAN_POINT('Ctrl Pts',(15.8,-13.626643760007,-4.77191579174908));
#12694=CARTESIAN_POINT('Ctrl Pts',(15.8,-13.6345795785203,-4.77539710335946));
#12695=CARTESIAN_POINT('Ctrl Pts',(10.0502525316942,-9.05620683581208,1.38781479615277));
#12696=CARTESIAN_POINT('Ctrl Pts',(11.9668350211294,-10.8374137839212,0.817330781359223));
#12697=CARTESIAN_POINT('Ctrl Pts',(13.8834175105647,-12.6186207320302,0.246846766565676));
#12698=CARTESIAN_POINT('Ctrl Pts',(15.8,-14.3998276801393,-0.32363724822787));
#12699=CARTESIAN_POINT('Ctrl Pts',(10.0502525316942,-9.21244502400637,1.39655842853148));
#12700=CARTESIAN_POINT('Ctrl Pts',(11.9668350211294,-11.0233696506194,0.813302761662288));
#12701=CARTESIAN_POINT('Ctrl Pts',(13.8834175105647,-12.8346197703481,0.230291956370553));
#12702=CARTESIAN_POINT('Ctrl Pts',(15.8,-14.6455443969611,-0.352963710498644));
#12703=CARTESIAN_POINT('Ctrl Pts',(10.0502525316942,-9.51829373400973,1.46541714813614));
#12704=CARTESIAN_POINT('Ctrl Pts',(11.9668350211295,-11.3925515672309,0.867231464171976));
#12705=CARTESIAN_POINT('Ctrl Pts',(13.8834175105647,-13.2668740653714,0.269566015193986));
#12706=CARTESIAN_POINT('Ctrl Pts',(15.8,-15.1411318985925,-0.32861966877018));
#12707=CARTESIAN_POINT('Ctrl Pts',(10.0502525316941,-10.0083300006652,1.79039750449509));
#12708=CARTESIAN_POINT('Ctrl Pts',(11.9668350211294,-12.0019243797287,1.20809631886684));
#12709=CARTESIAN_POINT('Ctrl Pts',(13.8834175105647,-13.9956114385882,0.625444427693871));
#12710=CARTESIAN_POINT('Ctrl Pts',(15.8,-15.9892058176518,0.0431432420656217));
#12711=CARTESIAN_POINT('Ctrl Pts',(10.0502525316942,-10.3276659549724,2.10732113862255));
#12712=CARTESIAN_POINT('Ctrl Pts',(11.9668350211294,-12.4074689224609,1.55295659524519));
#12713=CARTESIAN_POINT('Ctrl Pts',(13.8834175105647,-14.4874157824203,0.999648742962749));
#12714=CARTESIAN_POINT('Ctrl Pts',(15.8,-16.5672187499088,0.445284199585382));
#12715=CARTESIAN_POINT('Ctrl Pts',(10.0502525316942,-10.5073910450885,2.32206279789789));
#12716=CARTESIAN_POINT('Ctrl Pts',(11.9668350211294,-12.6387996550358,1.79024801807933));
#12717=CARTESIAN_POINT('Ctrl Pts',(13.8834175105647,-14.7702082649831,1.25843323826077));
#12718=CARTESIAN_POINT('Ctrl Pts',(15.8,-16.9016168749304,0.7266184584422));
#12719=CARTESIAN_POINT('',(10.0502525316942,-10.5073910450885,2.32206279789789));
#12720=CARTESIAN_POINT('',(15.8,-14.3998276801393,-0.32363724822787));
#12721=CARTESIAN_POINT('Ctrl Pts',(15.8,-14.3998276801393,-0.32363724822787));
#12722=CARTESIAN_POINT('Ctrl Pts',(15.4361339239126,-14.0704500021455,-0.216378749849824));
#12723=CARTESIAN_POINT('Ctrl Pts',(15.0706551397176,-13.7385848339403,-0.108278411513937));
#12724=CARTESIAN_POINT('Ctrl Pts',(14.7056733117528,-13.405863146671,8.83803447093712E-12));
#12725=CARTESIAN_POINT('Ctrl Pts',(15.8,-14.3998276801393,-0.32363724822787));
#12726=CARTESIAN_POINT('Ctrl Pts',(15.8,-14.4084472574799,-0.324666000821258));
#12727=CARTESIAN_POINT('Ctrl Pts',(15.8,-14.4170677396245,-0.325652230376828));
#12728=CARTESIAN_POINT('Ctrl Pts',(15.8,-14.4256891265865,-0.326595936941116));
#12729=CARTESIAN_POINT('Ctrl Pts',(15.8,-14.434311418564,-0.327497110819208));
#12730=CARTESIAN_POINT('Ctrl Pts',(15.8,-14.4429346149236,-0.328355732126618));
#12731=CARTESIAN_POINT('Ctrl Pts',(10.0502525316942,-8.18410616705958,4.11841212213242));
#12732=CARTESIAN_POINT('Ctrl Pts',(11.9668350211294,-10.0544238975194,4.12627279988524));
#12733=CARTESIAN_POINT('Ctrl Pts',(13.8834175105647,-11.9247416279792,4.13413347763806));
#12734=CARTESIAN_POINT('Ctrl Pts',(15.8,-13.795059358439,4.14199415539088));
#12735=CARTESIAN_POINT('Ctrl Pts',(10.0502525316942,-8.32999558303832,4.17500806600467));
#12736=CARTESIAN_POINT('Ctrl Pts',(11.9668350211294,-10.2325231628261,4.17990544851818));
#12737=CARTESIAN_POINT('Ctrl Pts',(13.8834175105647,-12.1352846385738,4.18513629113482));
#12738=CARTESIAN_POINT('Ctrl Pts',(15.8,-14.0378122183616,4.19003367364834));
#12739=CARTESIAN_POINT('Ctrl Pts',(10.0502525316942,-8.59959242261694,4.33502367302149));
#12740=CARTESIAN_POINT('Ctrl Pts',(11.9668350211295,-10.5669670902559,4.34529280263859));
#12741=CARTESIAN_POINT('Ctrl Pts',(13.8834175105647,-12.5342444956751,4.3560888733651));
#12742=CARTESIAN_POINT('Ctrl Pts',(15.8,-14.5016191633141,4.36635800298221));
#12743=CARTESIAN_POINT('Ctrl Pts',(10.0502525316941,-8.9652188127798,4.79552866926091));
#12744=CARTESIAN_POINT('Ctrl Pts',(11.9668350211294,-11.0411807000414,4.85778187524378));
#12745=CARTESIAN_POINT('Ctrl Pts',(13.8834175105647,-13.1173407686982,4.91974349130655));
#12746=CARTESIAN_POINT('Ctrl Pts',(15.8,-15.1933026559598,4.98199669728942));
#12747=CARTESIAN_POINT('Ctrl Pts',(10.0502525316942,-9.17099596015618,5.19560579312754));
#12748=CARTESIAN_POINT('Ctrl Pts',(11.9668350211294,-11.3203141899786,5.3110682436509));
#12749=CARTESIAN_POINT('Ctrl Pts',(13.8834175105647,-13.4694427341669,5.42758013234469));
#12750=CARTESIAN_POINT('Ctrl Pts',(15.8,-15.6187609639894,5.54304258286804));
#12751=CARTESIAN_POINT('Ctrl Pts',(10.0502525316942,-9.2755658561365,5.45537535466284));
#12752=CARTESIAN_POINT('Ctrl Pts',(11.9668350211294,-11.4669957083382,5.60823092528512));
#12753=CARTESIAN_POINT('Ctrl Pts',(13.8834175105647,-13.6584255605399,5.76108649590741));
#12754=CARTESIAN_POINT('Ctrl Pts',(15.8,-15.8498554127416,5.91394206652969));
#12755=CARTESIAN_POINT('',(10.0502525316942,-9.2755658561365,5.45537535466284));
#12756=CARTESIAN_POINT('',(15.8,-13.795059358439,4.14199415539088));
#12757=CARTESIAN_POINT('Ctrl Pts',(15.8,-13.795059358439,4.14199415539088));
#12758=CARTESIAN_POINT('Ctrl Pts',(15.5456574794164,-13.5529245928913,4.14215184549968));
#12759=CARTESIAN_POINT('Ctrl Pts',(15.2905267978562,-13.3095628770609,4.14233665870497));
#12760=CARTESIAN_POINT('Ctrl Pts',(15.0353288374156,-13.0655033718482,4.14249371366664));
#12761=CARTESIAN_POINT('Ctrl Pts',(14.7778805061931,-12.8192917162866,4.1426521535606));
#12762=CARTESIAN_POINT('Ctrl Pts',(14.5203637043096,-12.572369937213,4.14278210218064));
#12763=CARTESIAN_POINT('Ctrl Pts',(14.2635185530351,-12.3253345162694,4.14282007025482));
#12764=CARTESIAN_POINT('Ctrl Pts',(14.0000848089512,-12.0719621417566,4.14285901228618));
#12765=CARTESIAN_POINT('Ctrl Pts',(13.7373576158074,-11.8184702457667,4.14280091850188));
#12766=CARTESIAN_POINT('Ctrl Pts',(13.476135525203,-11.5655579735775,4.14257377376942));
#12767=CARTESIAN_POINT('Ctrl Pts',(13.2939617380614,-11.3891793743072,4.14241536520586));
#12768=CARTESIAN_POINT('Ctrl Pts',(13.1125199626836,-11.2130838733106,4.14217466317553));
#12769=CARTESIAN_POINT('Ctrl Pts',(12.9320810503802,-11.0375235228707,4.14182735974364));
#12770=CARTESIAN_POINT('Ctrl Pts',(12.7419408575533,-10.8525241873102,4.14146138357661));
#12771=CARTESIAN_POINT('Ctrl Pts',(12.5505199062851,-10.6658419590997,4.14098910290386));
#12772=CARTESIAN_POINT('Ctrl Pts',(12.3584607279937,-10.4779331330946,4.14033143664814));
#12773=CARTESIAN_POINT('Ctrl Pts',(12.1609502835666,-10.2846908414935,4.13965510367824));
#12774=CARTESIAN_POINT('Ctrl Pts',(11.9627648680236,-10.0901513147874,4.13878241284078));
#12775=CARTESIAN_POINT('Ctrl Pts',(11.7646032917777,-9.89486705366043,4.13762764472382));
#12776=CARTESIAN_POINT('Ctrl Pts',(11.5611710263552,-9.69438863400392,4.13644216215692));
#12777=CARTESIAN_POINT('Ctrl Pts',(11.3577638852471,-9.49312558221608,4.1349590374594));
#12778=CARTESIAN_POINT('Ctrl Pts',(11.1551379358829,-9.29173244420307,4.1330909916179));
#12779=CARTESIAN_POINT('Ctrl Pts',(10.9369434970465,-9.07486553810268,4.13107941701265));
#12780=CARTESIAN_POINT('Ctrl Pts',(10.7196549052601,-8.85784801697426,4.12862098831913));
#12781=CARTESIAN_POINT('Ctrl Pts',(10.5042162352556,-8.64155934493263,4.12562010893634));
#12782=CARTESIAN_POINT('Ctrl Pts',(10.3518584987053,-8.48860048887835,4.12349789387433));
#12783=CARTESIAN_POINT('Ctrl Pts',(10.2004259609779,-8.3360075858186,4.1211046936333));
#12784=CARTESIAN_POINT('Ctrl Pts',(10.0502525316942,-8.18410616705958,4.11841212213242));
#12785=CARTESIAN_POINT('Ctrl Pts',(15.8,-13.795059358439,4.14199415539088));
#12786=CARTESIAN_POINT('Ctrl Pts',(15.8,-13.8035749656708,4.14367934941586));
#12787=CARTESIAN_POINT('Ctrl Pts',(15.8,-13.8120782930811,4.14540526485286));
#12788=CARTESIAN_POINT('Ctrl Pts',(15.8,-13.8205693406969,4.14717190166177));
#12789=CARTESIAN_POINT('Ctrl Pts',(15.8,-13.8290481057107,4.14897926912419));
#12790=CARTESIAN_POINT('Ctrl Pts',(15.8,-13.8375145813754,4.15082738595568));
#12791=CARTESIAN_POINT('Ctrl Pts',(10.0502525316942,-6.51088816465466,6.44587057493322));
#12792=CARTESIAN_POINT('Ctrl Pts',(11.9668350211294,-8.28723694673789,7.03130648732539));
#12793=CARTESIAN_POINT('Ctrl Pts',(13.8834175105647,-10.0635857288211,7.61674239971757));
#12794=CARTESIAN_POINT('Ctrl Pts',(15.8,-11.8399345109044,8.20217831210975));
#12795=CARTESIAN_POINT('Ctrl Pts',(10.0502525316942,-6.63214813591052,6.54477882498566));
#12796=CARTESIAN_POINT('Ctrl Pts',(11.9668350211294,-8.4400460136743,7.13734986695939));
#12797=CARTESIAN_POINT('Ctrl Pts',(13.8834175105647,-10.2480632948761,7.73031032616364));
#12798=CARTESIAN_POINT('Ctrl Pts',(15.8,-12.0559611726399,8.32288136813736));
#12799=CARTESIAN_POINT('Ctrl Pts',(10.0502525316942,-6.83909882511009,6.78027814405441));
#12800=CARTESIAN_POINT('Ctrl Pts',(11.9668350211295,-8.70700998719297,7.39799687329663));
#12801=CARTESIAN_POINT('Ctrl Pts',(13.8834175105647,-10.5746650104356,8.01619193743949));
#12802=CARTESIAN_POINT('Ctrl Pts',(15.8,-12.4425761725185,8.6339106666817));
#12803=CARTESIAN_POINT('Ctrl Pts',(10.0502525316941,-7.04452561799895,7.33122941665115));
#12804=CARTESIAN_POINT('Ctrl Pts',(11.9668350211294,-8.99964539985646,8.03194323669995));
#12805=CARTESIAN_POINT('Ctrl Pts',(13.8834175105647,-10.9550426722922,8.73244671395173));
#12806=CARTESIAN_POINT('Ctrl Pts',(15.8,-12.9101624541497,9.43316053400054));
#12807=CARTESIAN_POINT('Ctrl Pts',(10.0502525316942,-7.11660498267375,7.77530835268703));
#12808=CARTESIAN_POINT('Ctrl Pts',(11.9668350211294,-9.12504823131445,8.54929552797968));
#12809=CARTESIAN_POINT('Ctrl Pts',(13.8834175105647,-11.1329867839675,9.32422216219831));
#12810=CARTESIAN_POINT('Ctrl Pts',(15.8,-13.1414300326082,10.098209337491));
#12811=CARTESIAN_POINT('Ctrl Pts',(10.0502525316942,-7.13578365451838,8.05467776187827));
#12812=CARTESIAN_POINT('Ctrl Pts',(11.9668350211294,-9.17272232645135,8.8772411146815));
#12813=CARTESIAN_POINT('Ctrl Pts',(13.8834175105647,-11.2096609983843,9.69980446748474));
#12814=CARTESIAN_POINT('Ctrl Pts',(15.8,-13.2465996703173,10.522367820288));
#12815=CARTESIAN_POINT('',(10.0502525316942,-7.13578365451838,8.05467776187827));
#12816=CARTESIAN_POINT('',(15.8,-11.8399345109044,8.20217831210975));
#12817=CARTESIAN_POINT('Ctrl Pts',(15.8,-11.8399345109044,8.20217831210975));
#12818=CARTESIAN_POINT('Ctrl Pts',(15.5456576615071,-11.6096021002865,8.12750458029304));
#12819=CARTESIAN_POINT('Ctrl Pts',(15.2905271631662,-11.3780944093856,8.05247749955213));
#12820=CARTESIAN_POINT('Ctrl Pts',(15.035329385525,-11.1459316587103,7.97720839274464));
#12821=CARTESIAN_POINT('Ctrl Pts',(14.77788119782,-10.9117216277044,7.90127554051966));
#12822=CARTESIAN_POINT('Ctrl Pts',(14.5203645390051,-10.6768450327863,7.82509615349662));
#12823=CARTESIAN_POINT('Ctrl Pts',(14.2635195291132,-10.4418887807051,7.74879417034763));
#12824=CARTESIAN_POINT('Ctrl Pts',(14.0000859949203,-10.2009054892931,7.67053490770775));
#12825=CARTESIAN_POINT('Ctrl Pts',(13.7373590095459,-9.95983851106062,7.59214642417425));
#12826=CARTESIAN_POINT('Ctrl Pts',(13.4761371226649,-9.71937502567191,7.51377627479595));
#12827=CARTESIAN_POINT('Ctrl Pts',(13.2939627987567,-9.5516774663352,7.45912147864529));
#12828=CARTESIAN_POINT('Ctrl Pts',(13.1125204900999,-9.38427458086327,7.40447589782802));
#12829=CARTESIAN_POINT('Ctrl Pts',(12.9320810503802,-9.21741359915303,7.34989430276011));
#12830=CARTESIAN_POINT('Ctrl Pts',(12.7419408661181,-9.04158187490351,7.29237830426415));
#12831=CARTESIAN_POINT('Ctrl Pts',(12.5505199235302,-8.86418247516742,7.23424116054649));
#12832=CARTESIAN_POINT('Ctrl Pts',(12.3584607539476,-8.68567379986618,7.17554866346896));
#12833=CARTESIAN_POINT('Ctrl Pts',(12.1609501017812,-8.50209826451042,7.11519021559974));
#12834=CARTESIAN_POINT('Ctrl Pts',(11.9627644770481,-8.31734966162796,7.0542441495787));
#12835=CARTESIAN_POINT('Ctrl Pts',(11.7646026923668,-8.13197994128604,6.99279967398786));
#12836=CARTESIAN_POINT('Ctrl Pts',(11.5611700299521,-7.94167959754981,6.92972084534173));
#12837=CARTESIAN_POINT('Ctrl Pts',(11.3577624926924,-7.75072500004995,6.86611647390365));
#12838=CARTESIAN_POINT('Ctrl Pts',(11.1551361524442,-7.55976563308342,6.80210582000276));
#12839=CARTESIAN_POINT('Ctrl Pts',(10.9369419552397,-7.35413478704973,6.73317720379554));
#12840=CARTESIAN_POINT('Ctrl Pts',(10.7196536056921,-7.14849878641203,6.66377706212369));
#12841=CARTESIAN_POINT('Ctrl Pts',(10.5042151754609,-6.94372358733556,6.59408624907876));
#12842=CARTESIAN_POINT('Ctrl Pts',(10.3518577964659,-6.79890721181244,6.54480112569497));
#12843=CARTESIAN_POINT('Ctrl Pts',(10.2004256127777,-6.65452261540817,6.49537136769543));
#12844=CARTESIAN_POINT('Ctrl Pts',(10.0502525316942,-6.51088816465466,6.44587057493322));
#12845=CARTESIAN_POINT('Ctrl Pts',(15.8,-11.8399345109044,8.20217831210975));
#12846=CARTESIAN_POINT('Ctrl Pts',(15.8,-11.8475125810599,8.20641249422049));
#12847=CARTESIAN_POINT('Ctrl Pts',(15.8,-11.8550663888027,8.21068161002192));
#12848=CARTESIAN_POINT('Ctrl Pts',(15.8,-11.862595934171,8.21498565948429));
#12849=CARTESIAN_POINT('Ctrl Pts',(15.8,-11.8701012116266,8.21932465056734));
#12850=CARTESIAN_POINT('Ctrl Pts',(15.8,-11.8775822089691,8.22369859898568));
#12851=CARTESIAN_POINT('Ctrl Pts',(10.0502525316942,-4.20033906466803,8.14236230483842));
#12852=CARTESIAN_POINT('Ctrl Pts',(11.9668350211294,-5.70883750303466,9.24806690579316));
#12853=CARTESIAN_POINT('Ctrl Pts',(13.8834175105647,-7.21733594140129,10.3537715067479));
#12854=CARTESIAN_POINT('Ctrl Pts',(15.8,-8.72583437976793,11.4594761077026));
#12855=CARTESIAN_POINT('Ctrl Pts',(10.0502525316942,-4.28509982034658,8.27390103242161));
#12856=CARTESIAN_POINT('Ctrl Pts',(11.9668350211294,-5.82139835544565,9.39614075158194));
#12857=CARTESIAN_POINT('Ctrl Pts',(13.8834175105647,-7.35769011342039,10.5187877262285));
#12858=CARTESIAN_POINT('Ctrl Pts',(15.8,-8.89398864851946,11.6410274453888));
#12859=CARTESIAN_POINT('Ctrl Pts',(10.0502525316942,-4.40914912230232,8.56182484570054));
#12860=CARTESIAN_POINT('Ctrl Pts',(11.9668350211295,-5.99475261978216,9.72652656145018));
#12861=CARTESIAN_POINT('Ctrl Pts',(13.8834175105647,-7.57996568930604,10.8916014121611));
#12862=CARTESIAN_POINT('Ctrl Pts',(15.8,-9.16556918678588,12.0563031279108));
#12863=CARTESIAN_POINT('Ctrl Pts',(10.0502525316941,-4.43426842278354,9.14929101108337));
#12864=CARTESIAN_POINT('Ctrl Pts',(11.9668350211294,-6.07716535286821,10.4198746943315));
#12865=CARTESIAN_POINT('Ctrl Pts',(13.8834175105647,-7.72039163021281,11.6903432820695));
#12866=CARTESIAN_POINT('Ctrl Pts',(15.8,-9.36328856029748,12.9609269653176));
#12867=CARTESIAN_POINT('Ctrl Pts',(10.0502525316942,-4.36559112518463,9.59390955692677));
#12868=CARTESIAN_POINT('Ctrl Pts',(11.9668350211294,-6.03655897381968,10.9506581995853));
#12869=CARTESIAN_POINT('Ctrl Pts',(13.8834175105647,-7.70675651927341,12.30814436114));
#12870=CARTESIAN_POINT('Ctrl Pts',(15.8,-9.37772436790846,13.6648930037986));
#12871=CARTESIAN_POINT('Ctrl Pts',(10.0502525316942,-4.29750123086779,9.86553218952113));
#12872=CARTESIAN_POINT('Ctrl Pts',(11.9668350211294,-5.98055897313701,11.2772850923971));
#12873=CARTESIAN_POINT('Ctrl Pts',(13.8834175105647,-7.66361671540623,12.689037995273));
#12874=CARTESIAN_POINT('Ctrl Pts',(15.8,-9.34667445767544,14.1007908981489));
#12875=CARTESIAN_POINT('',(10.0502525316942,-4.29750123086779,9.86553218952113));
#12876=CARTESIAN_POINT('',(15.8,-8.72583437976793,11.4594761077026));
#12877=CARTESIAN_POINT('Ctrl Pts',(15.8,-8.72583437976793,11.4594761077026));
#12878=CARTESIAN_POINT('Ctrl Pts',(15.5456576332007,-8.5298506700891,11.3172805234007));
#12879=CARTESIAN_POINT('Ctrl Pts',(15.2905271063779,-8.33285839341041,11.1743857021221));
#12880=CARTESIAN_POINT('Ctrl Pts',(15.0353293003201,-8.13531790820579,11.0310582754426));
#12881=CARTESIAN_POINT('Ctrl Pts',(14.7778810903262,-7.93603545706372,10.8864669483788));
#12882=CARTESIAN_POINT('Ctrl Pts',(14.5203644092921,-7.73619524960928,10.7414351729094));
#12883=CARTESIAN_POINT('Ctrl Pts',(14.2635193774431,-7.53631716809856,10.5962621862439));
#12884=CARTESIAN_POINT('Ctrl Pts',(14.0000858106901,-7.33131185594961,10.4473652525631));
#12885=CARTESIAN_POINT('Ctrl Pts',(13.7373587930849,-7.12626688447486,10.2983195619276));
#12886=CARTESIAN_POINT('Ctrl Pts',(13.4761368746011,-6.92179020337937,10.1494777981));
#12887=CARTESIAN_POINT('Ctrl Pts',(13.2939626340454,-6.77918967312477,10.0456766490784));
#12888=CARTESIAN_POINT('Ctrl Pts',(13.1125204081994,-6.63686654642574,9.94197532369136));
#12889=CARTESIAN_POINT('Ctrl Pts',(12.9320810503802,-6.49503902755748,9.83850230979699));
#12890=CARTESIAN_POINT('Ctrl Pts',(12.7419408648006,-6.34558654067311,9.72946635277443));
#12891=CARTESIAN_POINT('Ctrl Pts',(12.5505199208774,-6.19483505007998,9.61935521332108));
#12892=CARTESIAN_POINT('Ctrl Pts',(12.3584607499551,-6.04320018913773,9.50837311662927));
#12893=CARTESIAN_POINT('Ctrl Pts',(12.1609501300796,-5.88726129158013,9.39424088015534));
#12894=CARTESIAN_POINT('Ctrl Pts',(11.9627645378628,-5.73038832458536,9.27918728832947));
#12895=CARTESIAN_POINT('Ctrl Pts',(11.7646027855805,-5.57307865663081,9.16346774534079));
#12896=CARTESIAN_POINT('Ctrl Pts',(11.5611701848687,-5.41158475328911,9.04467021094158));
#12897=CARTESIAN_POINT('Ctrl Pts',(11.3577627091813,-5.24963101923067,8.92517068068734));
#12898=CARTESIAN_POINT('Ctrl Pts',(11.1551364296865,-5.08779829683614,8.80528327914573));
#12899=CARTESIAN_POINT('Ctrl Pts',(10.9369421951531,-4.91353182422761,8.67618482323567));
#12900=CARTESIAN_POINT('Ctrl Pts',(10.7196538081802,-4.73940615822464,8.54663632684897));
#12901=CARTESIAN_POINT('Ctrl Pts',(10.5042153409022,-4.56618898593296,8.41707738748288));
#12902=CARTESIAN_POINT('Ctrl Pts',(10.3518579060903,-4.44369032369707,8.32545369600313));
#12903=CARTESIAN_POINT('Ctrl Pts',(10.2004256671341,-4.32164700273153,8.23382587572327));
#12904=CARTESIAN_POINT('Ctrl Pts',(10.0502525316942,-4.20033906466803,8.14236230483842));
#12905=CARTESIAN_POINT('Ctrl Pts',(15.8,-8.72583437976793,11.4594761077026));
#12906=CARTESIAN_POINT('Ctrl Pts',(15.8,-8.73173311854078,11.4658448066529));
#12907=CARTESIAN_POINT('Ctrl Pts',(15.8,-8.73759798728384,11.4722392320194));
#12908=CARTESIAN_POINT('Ctrl Pts',(15.8,-8.74342898604263,11.4786593837858));
#12909=CARTESIAN_POINT('Ctrl Pts',(15.8,-8.7492261070902,11.4851052678107));
#12910=CARTESIAN_POINT('Ctrl Pts',(15.8,-8.7549893339674,11.4915768952696));
#12911=CARTESIAN_POINT('Ctrl Pts',(10.0502525316942,-1.47863151154858,9.041822881172));
#12912=CARTESIAN_POINT('Ctrl Pts',(11.9668350211294,-2.57161726872465,10.5595621004509));
#12913=CARTESIAN_POINT('Ctrl Pts',(13.8834175105647,-3.66460302590071,12.0773013197298));
#12914=CARTESIAN_POINT('Ctrl Pts',(15.8,-4.75758878307678,13.5950405390087));
#12915=CARTESIAN_POINT('Ctrl Pts',(10.0502525316942,-1.5185960783211,9.19311615914592));
#12916=CARTESIAN_POINT('Ctrl Pts',(11.9668350211294,-2.63291166611866,10.7351719126775));
#12917=CARTESIAN_POINT('Ctrl Pts',(13.8834175105647,-3.74709495962167,12.2776128949465));
#12918=CARTESIAN_POINT('Ctrl Pts',(15.8,-4.86141054741923,13.8196686484781));
#12919=CARTESIAN_POINT('Ctrl Pts',(10.0502525316942,-1.54760878347554,9.50527827631687));
#12920=CARTESIAN_POINT('Ctrl Pts',(11.9668350211295,-2.69569469846983,11.1029538596823));
#12921=CARTESIAN_POINT('Ctrl Pts',(13.8834175105647,-3.84329897549064,12.7008586295609));
#12922=CARTESIAN_POINT('Ctrl Pts',(15.8,-4.99138489048493,14.2985342129264));
#12923=CARTESIAN_POINT('Ctrl Pts',(10.0502525316941,-1.38996253959751,10.0717544060046));
#12924=CARTESIAN_POINT('Ctrl Pts',(11.9668350211294,-2.55981841965666,11.7878343688586));
#12925=CARTESIAN_POINT('Ctrl Pts',(13.8834175105647,-3.73002877331942,13.5039013178589));
#12926=CARTESIAN_POINT('Ctrl Pts',(15.8,-4.89988465337857,15.2199812807128));
#12927=CARTESIAN_POINT('Ctrl Pts',(10.0502525316942,-1.18724279150055,10.473392049036));
#12928=CARTESIAN_POINT('Ctrl Pts',(11.9668350211294,-2.35716926478797,12.2800941488934));
#12929=CARTESIAN_POINT('Ctrl Pts',(13.8834175105647,-3.52613523034269,14.0872596341291));
#12930=CARTESIAN_POINT('Ctrl Pts',(15.8,-4.69606170363011,15.8939617339865));
#12931=CARTESIAN_POINT('Ctrl Pts',(10.0502525316942,-1.03854944428814,10.7106795892491));
#12932=CARTESIAN_POINT('Ctrl Pts',(11.9668350211294,-2.20297683852746,12.5734298318033));
#12933=CARTESIAN_POINT('Ctrl Pts',(13.8834175105647,-3.36740423276678,14.4361800743576));
#12934=CARTESIAN_POINT('Ctrl Pts',(15.8,-4.5318316270061,16.2989303169119));
#12935=CARTESIAN_POINT('',(10.0502525316942,-1.03854944428814,10.7106795892491));
#12936=CARTESIAN_POINT('',(15.8,-4.75758878307678,13.5950405390087));
#12937=CARTESIAN_POINT('Ctrl Pts',(15.8,-4.75758878307678,13.5950405390087));
#12938=CARTESIAN_POINT('Ctrl Pts',(15.5456573899559,-4.61513791473816,13.3992420178034));
#12939=CARTESIAN_POINT('Ctrl Pts',(15.2905266183809,-4.47194392111073,13.2024668138653));
#12940=CARTESIAN_POINT('Ctrl Pts',(15.0353285681316,-4.32836223491271,13.0051107697455));
#12941=CARTESIAN_POINT('Ctrl Pts',(14.7778801662812,-4.18351443685719,12.8060144282785));
#12942=CARTESIAN_POINT('Ctrl Pts',(14.5203632939904,-4.03827228949013,12.6063268373516));
#12943=CARTESIAN_POINT('Ctrl Pts',(14.2635180731377,-3.89303775923429,12.4064932437282));
#12944=CARTESIAN_POINT('Ctrl Pts',(14.0000842255574,-3.74407765407913,12.201533492991));
#12945=CARTESIAN_POINT('Ctrl Pts',(13.7373569299619,-3.59512579987478,11.9964200114457));
#12946=CARTESIAN_POINT('Ctrl Pts',(13.4761347388995,-3.44665140507887,11.791676091236));
#12947=CARTESIAN_POINT('Ctrl Pts',(13.2939612159655,-3.34310697244292,11.6488899018536));
#12948=CARTESIAN_POINT('Ctrl Pts',(13.1125197030785,-3.23979551676186,11.5062843729564));
#12949=CARTESIAN_POINT('Ctrl Pts',(12.9320810503802,-3.13688485529761,11.3640491305165));
#12950=CARTESIAN_POINT('Ctrl Pts',(12.7419408532674,-3.02844105368856,11.2141664051166));
#12951=CARTESIAN_POINT('Ctrl Pts',(12.5505198976557,-2.91909407414947,11.0628597070358));
#12952=CARTESIAN_POINT('Ctrl Pts',(12.3584607150064,-2.80917609774746,10.9104517039517));
#12953=CARTESIAN_POINT('Ctrl Pts',(12.1609503726549,-2.69613835151589,10.7537179490171));
#12954=CARTESIAN_POINT('Ctrl Pts',(11.9627650599007,-2.5824969662107,10.5958192942301));
#12955=CARTESIAN_POINT('Ctrl Pts',(11.764603586073,-2.46864604141743,10.4371523366741));
#12956=CARTESIAN_POINT('Ctrl Pts',(11.5611715157472,-2.35176696854911,10.2742652373585));
#12957=CARTESIAN_POINT('Ctrl Pts',(11.357764569323,-2.23466749726805,10.1105684093218));
#12958=CARTESIAN_POINT('Ctrl Pts',(11.1551388120544,-2.1178029693577,9.94654008829807));
#12959=CARTESIAN_POINT('Ctrl Pts',(10.9369442531874,-1.99195912572037,9.76990860950719));
#12960=CARTESIAN_POINT('Ctrl Pts',(10.7196555410832,-1.86638826421775,9.59289262515015));
#12961=CARTESIAN_POINT('Ctrl Pts',(10.5042167520004,-1.74168466284082,9.41614744679526));
#12962=CARTESIAN_POINT('Ctrl Pts',(10.3518588411099,-1.65349450791466,9.29115358543552));
#12963=CARTESIAN_POINT('Ctrl Pts',(10.2004261307567,-1.5657386876737,9.16629650496035));
#12964=CARTESIAN_POINT('Ctrl Pts',(10.0502525316942,-1.47863151154858,9.041822881172));
#12965=CARTESIAN_POINT('Ctrl Pts',(15.8,-4.75758878307678,13.5950405390087));
#12966=CARTESIAN_POINT('Ctrl Pts',(15.8,-4.76123078081695,13.6029203421718));
#12967=CARTESIAN_POINT('Ctrl Pts',(15.8,-4.76483261634472,13.610814146196));
#12968=CARTESIAN_POINT('Ctrl Pts',(15.8,-4.7683942897085,13.6187219510797));
#12969=CARTESIAN_POINT('Ctrl Pts',(15.8,-4.77191579174908,13.626643760007));
#12970=CARTESIAN_POINT('Ctrl Pts',(15.8,-4.77539710335946,13.6345795785203));
#12971=CARTESIAN_POINT('Ctrl Pts',(10.0502525316942,1.38781479615277,9.05620683581208));
#12972=CARTESIAN_POINT('Ctrl Pts',(11.9668350211294,0.817330781359223,10.8374137839212));
#12973=CARTESIAN_POINT('Ctrl Pts',(13.8834175105647,0.246846766565676,12.6186207320303));
#12974=CARTESIAN_POINT('Ctrl Pts',(15.8,-0.323637248227871,14.3998276801393));
#12975=CARTESIAN_POINT('Ctrl Pts',(10.0502525316942,1.39655842853148,9.21244502400635));
#12976=CARTESIAN_POINT('Ctrl Pts',(11.9668350211294,0.813302761662287,11.0233696506194));
#12977=CARTESIAN_POINT('Ctrl Pts',(13.8834175105647,0.230291956370553,12.8346197703481));
#12978=CARTESIAN_POINT('Ctrl Pts',(15.8,-0.352963710498644,14.6455443969611));
#12979=CARTESIAN_POINT('Ctrl Pts',(10.0502525316942,1.46541714813613,9.51829373400972));
#12980=CARTESIAN_POINT('Ctrl Pts',(11.9668350211295,0.867231464171969,11.3925515672309));
#12981=CARTESIAN_POINT('Ctrl Pts',(13.8834175105647,0.269566015193983,13.2668740653713));
#12982=CARTESIAN_POINT('Ctrl Pts',(15.8,-0.328619668770181,15.1411318985925));
#12983=CARTESIAN_POINT('Ctrl Pts',(10.0502525316941,1.79039750449509,10.0083300006651));
#12984=CARTESIAN_POINT('Ctrl Pts',(11.9668350211294,1.20809631886684,12.0019243797287));
#12985=CARTESIAN_POINT('Ctrl Pts',(13.8834175105647,0.625444427693873,13.9956114385883));
#12986=CARTESIAN_POINT('Ctrl Pts',(15.7999999999999,0.043143242065623,15.9892058176518));
#12987=CARTESIAN_POINT('Ctrl Pts',(10.0502525316942,2.10732113862255,10.3276659549724));
#12988=CARTESIAN_POINT('Ctrl Pts',(11.9668350211294,1.55295659524519,12.4074689224609));
#12989=CARTESIAN_POINT('Ctrl Pts',(13.8834175105647,0.999648742962748,14.4874157824202));
#12990=CARTESIAN_POINT('Ctrl Pts',(15.8,0.445284199585382,16.5672187499087));
#12991=CARTESIAN_POINT('Ctrl Pts',(10.0502525316942,2.32206279789789,10.5073910450885));
#12992=CARTESIAN_POINT('Ctrl Pts',(11.9668350211294,1.79024801807933,12.6387996550358));
#12993=CARTESIAN_POINT('Ctrl Pts',(13.8834175105647,1.25843323826076,14.7702082649831));
#12994=CARTESIAN_POINT('Ctrl Pts',(15.8,0.7266184584422,16.9016168749304));
#12995=CARTESIAN_POINT('',(10.0502525316942,2.32206279789789,10.5073910450885));
#12996=CARTESIAN_POINT('',(15.8,-0.323637248227871,14.3998276801393));
#12997=CARTESIAN_POINT('Ctrl Pts',(15.8,-0.323637248227871,14.3998276801393));
#12998=CARTESIAN_POINT('Ctrl Pts',(15.5456570571827,-0.248663394075326,
14.1695921802541));
#12999=CARTESIAN_POINT('Ctrl Pts',(15.290525950772,-0.173284602939826,13.9381981568641));
#13000=CARTESIAN_POINT('Ctrl Pts',(15.0353275664542,-0.0977165877046862,
13.7061319160856));
#13001=CARTESIAN_POINT('Ctrl Pts',(14.7778789011685,-0.0214822309998696,
13.4720193682887));
#13002=CARTESIAN_POINT('Ctrl Pts',(14.5203617662622,0.0549444640636946,
13.23722264667));
#13003=CARTESIAN_POINT('Ctrl Pts',(14.2635162858845,0.131318796804616,13.0022894235191));
#13004=CARTESIAN_POINT('Ctrl Pts',(14.0000820510512,0.209652329779073,12.7613295522896));
#13005=CARTESIAN_POINT('Ctrl Pts',(13.737354372103,0.287930509546182,12.5202260255198));
#13006=CARTESIAN_POINT('Ctrl Pts',(13.4761318051391,0.365868800886513,12.2796215208081));
#13007=CARTESIAN_POINT('Ctrl Pts',(13.2939592679841,0.420221747647607,12.1118276981546));
#13008=CARTESIAN_POINT('Ctrl Pts',(13.1125187344712,0.474408950394415,11.9442776868956));
#13009=CARTESIAN_POINT('Ctrl Pts',(12.9320810503802,0.528329405335826,11.7772036867065));
#13010=CARTESIAN_POINT('Ctrl Pts',(12.7419408368634,0.58514928122335,11.6011457516411));
#13011=CARTESIAN_POINT('Ctrl Pts',(12.5505198646266,0.642388101081342,11.4234544410913));
#13012=CARTESIAN_POINT('Ctrl Pts',(12.3584606652976,0.69982965272817,11.2445392798291));
#13013=CARTESIAN_POINT('Ctrl Pts',(12.1609507027355,0.758901432444593,11.0605463915626));
#13014=CARTESIAN_POINT('Ctrl Pts',(11.9627657724259,0.818187336020824,10.8752590885166));
#13015=CARTESIAN_POINT('Ctrl Pts',(11.7646046796656,0.877435109078001,10.6891763370127));
#13016=CARTESIAN_POINT('Ctrl Pts',(11.5611733354004,0.938258623673378,10.498144567074));
#13017=CARTESIAN_POINT('Ctrl Pts',(11.3577671135027,0.999041534288953,10.3062745975178));
#13018=CARTESIAN_POINT('Ctrl Pts',(11.1551420711301,1.05949856916745,10.1141619588682));
#13019=CARTESIAN_POINT('Ctrl Pts',(10.9369470578872,1.12460120096202,9.90728713607513));
#13020=CARTESIAN_POINT('Ctrl Pts',(10.7196578904047,1.18932539513682,9.70013097729772));
#13021=CARTESIAN_POINT('Ctrl Pts',(10.5042186507217,1.25330845309555,9.49350036754161));
#13022=CARTESIAN_POINT('Ctrl Pts',(10.3518600992373,1.29855724827547,9.34737127591884));
#13023=CARTESIAN_POINT('Ctrl Pts',(10.20042675459,1.3434352294294,9.20150648816153));
#13024=CARTESIAN_POINT('Ctrl Pts',(10.0502525316942,1.38781479615277,9.05620683581208));
#13025=CARTESIAN_POINT('Ctrl Pts',(15.8,-0.323637248227871,14.3998276801393));
#13026=CARTESIAN_POINT('Ctrl Pts',(15.8,-0.324666000821258,14.4084472574799));
#13027=CARTESIAN_POINT('Ctrl Pts',(15.8,-0.325652230376828,14.4170677396245));
#13028=CARTESIAN_POINT('Ctrl Pts',(15.8,-0.326595936941117,14.4256891265865));
#13029=CARTESIAN_POINT('Ctrl Pts',(15.8,-0.327497110819209,14.434311418564));
#13030=CARTESIAN_POINT('Ctrl Pts',(15.8,-0.328355732126619,14.4429346149236));
#13031=CARTESIAN_POINT('Ctrl Pts',(10.0502525316942,4.11841212213242,8.18410616705958));
#13032=CARTESIAN_POINT('Ctrl Pts',(11.9668350211294,4.12627279988524,10.0544238975194));
#13033=CARTESIAN_POINT('Ctrl Pts',(13.8834175105647,4.13413347763806,11.9247416279792));
#13034=CARTESIAN_POINT('Ctrl Pts',(15.8,4.14199415539088,13.795059358439));
#13035=CARTESIAN_POINT('Ctrl Pts',(10.0502525316942,4.17500806600467,8.3299955830383));
#13036=CARTESIAN_POINT('Ctrl Pts',(11.9668350211294,4.17990544851818,10.2325231628261));
#13037=CARTESIAN_POINT('Ctrl Pts',(13.8834175105647,4.18513629113481,12.1352846385738));
#13038=CARTESIAN_POINT('Ctrl Pts',(15.8,4.19003367364832,14.0378122183616));
#13039=CARTESIAN_POINT('Ctrl Pts',(10.0502525316942,4.3350236730215,8.59959242261694));
#13040=CARTESIAN_POINT('Ctrl Pts',(11.9668350211295,4.34529280263861,10.5669670902559));
#13041=CARTESIAN_POINT('Ctrl Pts',(13.8834175105647,4.35608887336509,12.5342444956751));
#13042=CARTESIAN_POINT('Ctrl Pts',(15.8,4.36635800298219,14.501619163314));
#13043=CARTESIAN_POINT('Ctrl Pts',(10.0502525316941,4.79552866926089,8.96521881277978));
#13044=CARTESIAN_POINT('Ctrl Pts',(11.9668350211294,4.85778187524376,11.0411807000414));
#13045=CARTESIAN_POINT('Ctrl Pts',(13.8834175105647,4.91974349130654,13.1173407686982));
#13046=CARTESIAN_POINT('Ctrl Pts',(15.8,4.98199669728941,15.1933026559598));
#13047=CARTESIAN_POINT('Ctrl Pts',(10.0502525316942,5.19560579312754,9.17099596015618));
#13048=CARTESIAN_POINT('Ctrl Pts',(11.9668350211294,5.3110682436509,11.3203141899786));
#13049=CARTESIAN_POINT('Ctrl Pts',(13.8834175105647,5.42758013234466,13.4694427341669));
#13050=CARTESIAN_POINT('Ctrl Pts',(15.8,5.54304258286802,15.6187609639894));
#13051=CARTESIAN_POINT('Ctrl Pts',(10.0502525316942,5.45537535466284,9.2755658561365));
#13052=CARTESIAN_POINT('Ctrl Pts',(11.9668350211294,5.60823092528512,11.4669957083382));
#13053=CARTESIAN_POINT('Ctrl Pts',(13.8834175105647,5.76108649590741,13.6584255605399));
#13054=CARTESIAN_POINT('Ctrl Pts',(15.8,5.91394206652969,15.8498554127416));
#13055=CARTESIAN_POINT('',(10.0502525316942,5.45537535466284,9.2755658561365));
#13056=CARTESIAN_POINT('',(15.8,4.14199415539088,13.795059358439));
#13057=CARTESIAN_POINT('Ctrl Pts',(15.8,4.14199415539088,13.795059358439));
#13058=CARTESIAN_POINT('Ctrl Pts',(15.5456574794166,4.14215184549968,13.5529245928915));
#13059=CARTESIAN_POINT('Ctrl Pts',(15.2905267978567,4.14233665870497,13.3095628770614));
#13060=CARTESIAN_POINT('Ctrl Pts',(15.0353288374163,4.14249371366664,13.0655033718489));
#13061=CARTESIAN_POINT('Ctrl Pts',(14.7778805061933,4.1426521535606,12.8192917162869));
#13062=CARTESIAN_POINT('Ctrl Pts',(14.5203637043094,4.14278210218064,12.5723699372128));
#13063=CARTESIAN_POINT('Ctrl Pts',(14.2635185530345,4.14282007025482,12.3253345162688));
#13064=CARTESIAN_POINT('Ctrl Pts',(14.0000848089498,4.14285901228618,12.0719621417552));
#13065=CARTESIAN_POINT('Ctrl Pts',(13.7373576158051,4.14280091850188,11.8184702457645));
#13066=CARTESIAN_POINT('Ctrl Pts',(13.4761355251999,4.14257377376941,11.5655579735746));
#13067=CARTESIAN_POINT('Ctrl Pts',(13.2939617380594,4.14241536520585,11.3891793743052));
#13068=CARTESIAN_POINT('Ctrl Pts',(13.1125199626826,4.14217466317552,11.2130838733096));
#13069=CARTESIAN_POINT('Ctrl Pts',(12.9320810503802,4.14182735974364,11.0375235228707));
#13070=CARTESIAN_POINT('Ctrl Pts',(12.7419408575531,4.14146138357661,10.85252418731));
#13071=CARTESIAN_POINT('Ctrl Pts',(12.5505199062848,4.14098910290385,10.6658419590994));
#13072=CARTESIAN_POINT('Ctrl Pts',(12.3584607279933,4.14033143664814,10.4779331330941));
#13073=CARTESIAN_POINT('Ctrl Pts',(12.160950283566,4.13965510367824,10.2846908414929));
#13074=CARTESIAN_POINT('Ctrl Pts',(11.962764868023,4.13878241284077,10.0901513147869));
#13075=CARTESIAN_POINT('Ctrl Pts',(11.7646032917771,4.13762764472382,9.89486705365981));
#13076=CARTESIAN_POINT('Ctrl Pts',(11.5611710263546,4.13644216215692,9.69438863400336));
#13077=CARTESIAN_POINT('Ctrl Pts',(11.3577638852466,4.13495903745939,9.49312558221559));
#13078=CARTESIAN_POINT('Ctrl Pts',(11.1551379358825,4.1330909916179,9.29173244420265));
#13079=CARTESIAN_POINT('Ctrl Pts',(10.9369434970461,4.13107941701264,9.07486553810229));
#13080=CARTESIAN_POINT('Ctrl Pts',(10.7196549052597,4.12862098831913,8.85784801697389));
#13081=CARTESIAN_POINT('Ctrl Pts',(10.5042162352553,4.12562010893634,8.6415593449323));
#13082=CARTESIAN_POINT('Ctrl Pts',(10.3518584987051,4.12349789387433,8.48860048887813));
#13083=CARTESIAN_POINT('Ctrl Pts',(10.2004259609778,4.12110469363329,8.33600758581849));
#13084=CARTESIAN_POINT('Ctrl Pts',(10.0502525316942,4.11841212213242,8.18410616705958));
#13085=CARTESIAN_POINT('Ctrl Pts',(15.8,4.14199415539088,13.795059358439));
#13086=CARTESIAN_POINT('Ctrl Pts',(15.8,4.14367934941586,13.8035749656708));
#13087=CARTESIAN_POINT('Ctrl Pts',(15.8,4.14540526485285,13.8120782930811));
#13088=CARTESIAN_POINT('Ctrl Pts',(15.8,4.14717190166176,13.8205693406969));
#13089=CARTESIAN_POINT('Ctrl Pts',(15.8,4.14897926912419,13.8290481057107));
#13090=CARTESIAN_POINT('Ctrl Pts',(15.8,4.15082738595568,13.8375145813754));
#13091=CARTESIAN_POINT('Ctrl Pts',(10.0502525316942,6.44587057493322,6.51088816465466));
#13092=CARTESIAN_POINT('Ctrl Pts',(11.9668350211294,7.03130648732539,8.28723694673789));
#13093=CARTESIAN_POINT('Ctrl Pts',(13.8834175105647,7.61674239971757,10.0635857288211));
#13094=CARTESIAN_POINT('Ctrl Pts',(15.8,8.20217831210975,11.8399345109044));
#13095=CARTESIAN_POINT('Ctrl Pts',(10.0502525316942,6.54477882498566,6.6321481359105));
#13096=CARTESIAN_POINT('Ctrl Pts',(11.9668350211294,7.13734986695938,8.44004601367429));
#13097=CARTESIAN_POINT('Ctrl Pts',(13.8834175105647,7.73031032616364,10.2480632948761));
#13098=CARTESIAN_POINT('Ctrl Pts',(15.8,8.32288136813736,12.0559611726399));
#13099=CARTESIAN_POINT('Ctrl Pts',(10.0502525316942,6.78027814405439,6.83909882511009));
#13100=CARTESIAN_POINT('Ctrl Pts',(11.9668350211295,7.39799687329661,8.70700998719296));
#13101=CARTESIAN_POINT('Ctrl Pts',(13.8834175105647,8.01619193743947,10.5746650104356));
#13102=CARTESIAN_POINT('Ctrl Pts',(15.8,8.63391066668169,12.4425761725185));
#13103=CARTESIAN_POINT('Ctrl Pts',(10.0502525316941,7.33122941665113,7.04452561799896));
#13104=CARTESIAN_POINT('Ctrl Pts',(11.9668350211294,8.03194323669993,8.99964539985647));
#13105=CARTESIAN_POINT('Ctrl Pts',(13.8834175105647,8.73244671395173,10.9550426722922));
#13106=CARTESIAN_POINT('Ctrl Pts',(15.8,9.43316053400053,12.9101624541498));
#13107=CARTESIAN_POINT('Ctrl Pts',(10.0502525316942,7.77530835268703,7.11660498267373));
#13108=CARTESIAN_POINT('Ctrl Pts',(11.9668350211294,8.54929552797968,9.12504823131443));
#13109=CARTESIAN_POINT('Ctrl Pts',(13.8834175105647,9.32422216219826,11.1329867839676));
#13110=CARTESIAN_POINT('Ctrl Pts',(15.8,10.0982093374909,13.1414300326083));
#13111=CARTESIAN_POINT('Ctrl Pts',(10.0502525316942,8.05467776187827,7.13578365451838));
#13112=CARTESIAN_POINT('Ctrl Pts',(11.9668350211294,8.8772411146815,9.17272232645135));
#13113=CARTESIAN_POINT('Ctrl Pts',(13.8834175105647,9.69980446748474,11.2096609983843));
#13114=CARTESIAN_POINT('Ctrl Pts',(15.8,10.522367820288,13.2465996703173));
#13115=CARTESIAN_POINT('',(10.0502525316942,8.05467776187827,7.13578365451838));
#13116=CARTESIAN_POINT('',(15.8,8.20217831210975,11.8399345109044));
#13117=CARTESIAN_POINT('Ctrl Pts',(15.8,8.20217831210975,11.8399345109044));
#13118=CARTESIAN_POINT('Ctrl Pts',(15.5456576615066,8.1275045802929,11.6096021002861));
#13119=CARTESIAN_POINT('Ctrl Pts',(15.2905271631652,8.05247749955186,11.3780944093847));
#13120=CARTESIAN_POINT('Ctrl Pts',(15.0353293855237,7.97720839274424,11.1459316587091));
#13121=CARTESIAN_POINT('Ctrl Pts',(14.7778811978186,7.90127554051927,10.9117216277032));
#13122=CARTESIAN_POINT('Ctrl Pts',(14.5203645390038,7.82509615349623,10.6768450327852));
#13123=CARTESIAN_POINT('Ctrl Pts',(14.263519529112,7.74879417034726,10.441888780704));
#13124=CARTESIAN_POINT('Ctrl Pts',(14.0000859949182,7.67053490770714,10.2009054892912));
#13125=CARTESIAN_POINT('Ctrl Pts',(13.7373590095431,7.5921464241734,9.959838511058));
#13126=CARTESIAN_POINT('Ctrl Pts',(13.4761371226612,7.51377627479485,9.71937502566857));
#13127=CARTESIAN_POINT('Ctrl Pts',(13.2939627987543,7.45912147864456,9.55167746633298));
#13128=CARTESIAN_POINT('Ctrl Pts',(13.1125204900987,7.40447589782765,9.38427458086216));
#13129=CARTESIAN_POINT('Ctrl Pts',(12.9320810503802,7.3498943027601,9.21741359915303));
#13130=CARTESIAN_POINT('Ctrl Pts',(12.7419408661186,7.29237830426429,9.04158187490393));
#13131=CARTESIAN_POINT('Ctrl Pts',(12.5505199235311,7.23424116054677,8.86418247516826));
#13132=CARTESIAN_POINT('Ctrl Pts',(12.3584607539489,7.17554866346938,8.68567379986745));
#13133=CARTESIAN_POINT('Ctrl Pts',(12.1609501017825,7.11519021560016,8.5020982645117));
#13134=CARTESIAN_POINT('Ctrl Pts',(11.9627644770495,7.05424414957912,8.31734966162925));
#13135=CARTESIAN_POINT('Ctrl Pts',(11.7646026923682,6.99279967398829,8.13197994128733));
#13136=CARTESIAN_POINT('Ctrl Pts',(11.5611700299535,6.92972084534216,7.94167959755111));
#13137=CARTESIAN_POINT('Ctrl Pts',(11.3577624926938,6.86611647390408,7.75072500005124));
#13138=CARTESIAN_POINT('Ctrl Pts',(11.1551361524456,6.80210582000319,7.55976563308471));
#13139=CARTESIAN_POINT('Ctrl Pts',(10.9369419552409,6.73317720379591,7.35413478705085));
#13140=CARTESIAN_POINT('Ctrl Pts',(10.7196536056931,6.66377706212401,7.14849878641298));
#13141=CARTESIAN_POINT('Ctrl Pts',(10.5042151754617,6.59408624907902,6.94372358733632));
#13142=CARTESIAN_POINT('Ctrl Pts',(10.3518577964665,6.54480112569514,6.79890721181295));
#13143=CARTESIAN_POINT('Ctrl Pts',(10.2004256127779,6.49537136769551,6.65452261540843));
#13144=CARTESIAN_POINT('Ctrl Pts',(10.0502525316942,6.44587057493322,6.51088816465466));
#13145=CARTESIAN_POINT('Ctrl Pts',(15.8,8.20217831210975,11.8399345109044));
#13146=CARTESIAN_POINT('Ctrl Pts',(15.8,8.20641249422049,11.8475125810599));
#13147=CARTESIAN_POINT('Ctrl Pts',(15.8,8.21068161002192,11.8550663888027));
#13148=CARTESIAN_POINT('Ctrl Pts',(15.8,8.21498565948429,11.862595934171));
#13149=CARTESIAN_POINT('Ctrl Pts',(15.8,8.21932465056733,11.8701012116266));
#13150=CARTESIAN_POINT('Ctrl Pts',(15.8,8.22369859898568,11.8775822089691));
#13151=CARTESIAN_POINT('Ctrl Pts',(10.0502525316942,8.14236230483842,4.20033906466803));
#13152=CARTESIAN_POINT('Ctrl Pts',(11.9668350211294,9.24806690579316,5.70883750303466));
#13153=CARTESIAN_POINT('Ctrl Pts',(13.8834175105647,10.3537715067479,7.2173359414013));
#13154=CARTESIAN_POINT('Ctrl Pts',(15.8,11.4594761077026,8.72583437976793));
#13155=CARTESIAN_POINT('Ctrl Pts',(10.0502525316942,8.27390103242162,4.28509982034658));
#13156=CARTESIAN_POINT('Ctrl Pts',(11.9668350211294,9.39614075158195,5.82139835544565));
#13157=CARTESIAN_POINT('Ctrl Pts',(13.8834175105647,10.5187877262285,7.35769011342039));
#13158=CARTESIAN_POINT('Ctrl Pts',(15.8,11.6410274453888,8.89398864851946));
#13159=CARTESIAN_POINT('Ctrl Pts',(10.0502525316942,8.56182484570054,4.40914912230233));
#13160=CARTESIAN_POINT('Ctrl Pts',(11.9668350211295,9.72652656145018,5.99475261978217));
#13161=CARTESIAN_POINT('Ctrl Pts',(13.8834175105647,10.8916014121612,7.57996568930602));
#13162=CARTESIAN_POINT('Ctrl Pts',(15.8,12.0563031279108,9.16556918678585));
#13163=CARTESIAN_POINT('Ctrl Pts',(10.0502525316941,9.14929101108338,4.43426842278356));
#13164=CARTESIAN_POINT('Ctrl Pts',(11.9668350211294,10.4198746943315,6.07716535286823));
#13165=CARTESIAN_POINT('Ctrl Pts',(13.8834175105647,11.6903432820694,7.72039163021277));
#13166=CARTESIAN_POINT('Ctrl Pts',(15.8,12.9609269653175,9.36328856029745));
#13167=CARTESIAN_POINT('Ctrl Pts',(10.0502525316942,9.59390955692677,4.36559112518463));
#13168=CARTESIAN_POINT('Ctrl Pts',(11.9668350211294,10.9506581995853,6.03655897381968));
#13169=CARTESIAN_POINT('Ctrl Pts',(13.8834175105647,12.30814436114,7.70675651927344));
#13170=CARTESIAN_POINT('Ctrl Pts',(15.8,13.6648930037986,9.37772436790849));
#13171=CARTESIAN_POINT('Ctrl Pts',(10.0502525316942,9.86553218952113,4.2975012308678));
#13172=CARTESIAN_POINT('Ctrl Pts',(11.9668350211294,11.2772850923971,5.98055897313701));
#13173=CARTESIAN_POINT('Ctrl Pts',(13.8834175105647,12.689037995273,7.66361671540623));
#13174=CARTESIAN_POINT('Ctrl Pts',(15.8,14.1007908981489,9.34667445767544));
#13175=CARTESIAN_POINT('',(10.0502525316942,9.86553218952113,4.2975012308678));
#13176=CARTESIAN_POINT('',(15.8,11.4594761077026,8.72583437976793));
#13177=CARTESIAN_POINT('Ctrl Pts',(15.8,11.4594761077026,8.72583437976793));
#13178=CARTESIAN_POINT('Ctrl Pts',(15.5456576332005,11.3172805234006,8.52985067008894));
#13179=CARTESIAN_POINT('Ctrl Pts',(15.2905271063775,11.1743857021219,8.33285839341008));
#13180=CARTESIAN_POINT('Ctrl Pts',(15.0353293003195,11.0310582754423,8.13531790820529));
#13181=CARTESIAN_POINT('Ctrl Pts',(14.7778810903258,10.8864669483786,7.93603545706342));
#13182=CARTESIAN_POINT('Ctrl Pts',(14.520364409292,10.7414351729093,7.73619524960918));
#13183=CARTESIAN_POINT('Ctrl Pts',(14.2635193774432,10.596262186244,7.53631716809864));
#13184=CARTESIAN_POINT('Ctrl Pts',(14.0000858106889,10.4473652525624,7.3313118559487));
#13185=CARTESIAN_POINT('Ctrl Pts',(13.7373587930825,10.2983195619262,7.12626688447295));
#13186=CARTESIAN_POINT('Ctrl Pts',(13.4761368745974,10.1494777980979,6.92179020337647));
#13187=CARTESIAN_POINT('Ctrl Pts',(13.2939626340429,10.045676649077,6.77918967312285));
#13188=CARTESIAN_POINT('Ctrl Pts',(13.1125204081982,9.94197532369066,6.63686654642478));
#13189=CARTESIAN_POINT('Ctrl Pts',(12.9320810503802,9.83850230979699,6.49503902755748));
#13190=CARTESIAN_POINT('Ctrl Pts',(12.7419408648006,9.72946635277444,6.34558654067312));
#13191=CARTESIAN_POINT('Ctrl Pts',(12.5505199208775,9.6193552133211,6.19483505008001));
#13192=CARTESIAN_POINT('Ctrl Pts',(12.3584607499552,9.50837311662931,6.04320018913779));
#13193=CARTESIAN_POINT('Ctrl Pts',(12.1609501300795,9.39424088015531,5.88726129158008));
#13194=CARTESIAN_POINT('Ctrl Pts',(11.9627645378627,9.27918728832936,5.73038832458522));
#13195=CARTESIAN_POINT('Ctrl Pts',(11.7646027855802,9.16346774534062,5.57307865663058));
#13196=CARTESIAN_POINT('Ctrl Pts',(11.5611701848685,9.04467021094143,5.4115847532889));
#13197=CARTESIAN_POINT('Ctrl Pts',(11.3577627091811,8.92517068068721,5.2496310192305));
#13198=CARTESIAN_POINT('Ctrl Pts',(11.1551364296864,8.80528327914564,5.087798296836));
#13199=CARTESIAN_POINT('Ctrl Pts',(10.9369421951531,8.67618482323568,4.91353182422764));
#13200=CARTESIAN_POINT('Ctrl Pts',(10.7196538081805,8.5466363268491,4.73940615822481));
#13201=CARTESIAN_POINT('Ctrl Pts',(10.5042153409026,8.41707738748313,4.5661889859333));
#13202=CARTESIAN_POINT('Ctrl Pts',(10.3518579060906,8.32545369600329,4.44369032369729));
#13203=CARTESIAN_POINT('Ctrl Pts',(10.2004256671343,8.23382587572336,4.32164700273164));
#13204=CARTESIAN_POINT('Ctrl Pts',(10.0502525316942,8.14236230483842,4.20033906466803));
#13205=CARTESIAN_POINT('Ctrl Pts',(15.8,11.4594761077026,8.72583437976793));
#13206=CARTESIAN_POINT('Ctrl Pts',(15.8,11.4658448066529,8.73173311854078));
#13207=CARTESIAN_POINT('Ctrl Pts',(15.8,11.4722392320194,8.73759798728384));
#13208=CARTESIAN_POINT('Ctrl Pts',(15.8,11.4786593837858,8.74342898604263));
#13209=CARTESIAN_POINT('Ctrl Pts',(15.8,11.4851052678107,8.74922610709021));
#13210=CARTESIAN_POINT('Ctrl Pts',(15.8,11.4915768952696,8.7549893339674));
#13211=CARTESIAN_POINT('Ctrl Pts',(10.0502525316942,9.041822881172,1.47863151154858));
#13212=CARTESIAN_POINT('Ctrl Pts',(11.9668350211294,10.5595621004509,2.57161726872465));
#13213=CARTESIAN_POINT('Ctrl Pts',(13.8834175105647,12.0773013197298,3.66460302590071));
#13214=CARTESIAN_POINT('Ctrl Pts',(15.8,13.5950405390087,4.75758878307678));
#13215=CARTESIAN_POINT('Ctrl Pts',(10.0502525316942,9.19311615914592,1.5185960783211));
#13216=CARTESIAN_POINT('Ctrl Pts',(11.9668350211294,10.7351719126775,2.63291166611866));
#13217=CARTESIAN_POINT('Ctrl Pts',(13.8834175105647,12.2776128949465,3.74709495962168));
#13218=CARTESIAN_POINT('Ctrl Pts',(15.8,13.8196686484781,4.86141054741924));
#13219=CARTESIAN_POINT('Ctrl Pts',(10.0502525316942,9.50527827631687,1.54760878347554));
#13220=CARTESIAN_POINT('Ctrl Pts',(11.9668350211295,11.1029538596823,2.69569469846983));
#13221=CARTESIAN_POINT('Ctrl Pts',(13.8834175105647,12.7008586295609,3.84329897549064));
#13222=CARTESIAN_POINT('Ctrl Pts',(15.8,14.2985342129264,4.99138489048493));
#13223=CARTESIAN_POINT('Ctrl Pts',(10.0502525316941,10.0717544060046,1.38996253959751));
#13224=CARTESIAN_POINT('Ctrl Pts',(11.9668350211294,11.7878343688586,2.55981841965666));
#13225=CARTESIAN_POINT('Ctrl Pts',(13.8834175105647,13.5039013178589,3.73002877331941));
#13226=CARTESIAN_POINT('Ctrl Pts',(15.8,15.2199812807128,4.89988465337857));
#13227=CARTESIAN_POINT('Ctrl Pts',(10.0502525316942,10.473392049036,1.18724279150055));
#13228=CARTESIAN_POINT('Ctrl Pts',(11.9668350211294,12.2800941488934,2.35716926478797));
#13229=CARTESIAN_POINT('Ctrl Pts',(13.8834175105647,14.0872596341291,3.52613523034269));
#13230=CARTESIAN_POINT('Ctrl Pts',(15.8,15.8939617339865,4.69606170363011));
#13231=CARTESIAN_POINT('Ctrl Pts',(10.0502525316942,10.7106795892491,1.03854944428815));
#13232=CARTESIAN_POINT('Ctrl Pts',(11.9668350211294,12.5734298318033,2.20297683852746));
#13233=CARTESIAN_POINT('Ctrl Pts',(13.8834175105647,14.4361800743576,3.36740423276678));
#13234=CARTESIAN_POINT('Ctrl Pts',(15.8,16.2989303169119,4.5318316270061));
#13235=CARTESIAN_POINT('',(10.0502525316942,10.7106795892491,1.03854944428815));
#13236=CARTESIAN_POINT('',(15.8,13.5950405390087,4.75758878307678));
#13237=CARTESIAN_POINT('Ctrl Pts',(15.8,13.5950405390087,4.75758878307678));
#13238=CARTESIAN_POINT('Ctrl Pts',(15.5456573899564,13.3992420178037,4.61513791473842));
#13239=CARTESIAN_POINT('Ctrl Pts',(15.2905266183818,13.202466813866,4.47194392111128));
#13240=CARTESIAN_POINT('Ctrl Pts',(15.0353285681331,13.0051107697467,4.32836223491354));
#13241=CARTESIAN_POINT('Ctrl Pts',(14.7778801662818,12.806014428279,4.18351443685758));
#13242=CARTESIAN_POINT('Ctrl Pts',(14.5203632939903,12.6063268373515,4.03827228949007));
#13243=CARTESIAN_POINT('Ctrl Pts',(14.2635180731369,12.4064932437275,3.8930377592338));
#13244=CARTESIAN_POINT('Ctrl Pts',(14.000084225555,12.2015334929891,3.74407765407776));
#13245=CARTESIAN_POINT('Ctrl Pts',(13.7373569299579,11.9964200114426,3.59512579987254));
#13246=CARTESIAN_POINT('Ctrl Pts',(13.476134738894,11.7916760912317,3.44665140507575));
#13247=CARTESIAN_POINT('Ctrl Pts',(13.2939612159618,11.6488899018507,3.34310697244085));
#13248=CARTESIAN_POINT('Ctrl Pts',(13.1125197030766,11.5062843729549,3.23979551676083));
#13249=CARTESIAN_POINT('Ctrl Pts',(12.9320810503802,11.3640491305165,3.13688485529761));
#13250=CARTESIAN_POINT('Ctrl Pts',(12.7419408532675,11.2141664051166,3.02844105368859));
#13251=CARTESIAN_POINT('Ctrl Pts',(12.5505198976558,11.0628597070359,2.91909407414952));
#13252=CARTESIAN_POINT('Ctrl Pts',(12.3584607150066,10.9104517039518,2.80917609774754));
#13253=CARTESIAN_POINT('Ctrl Pts',(12.160950372655,10.7537179490173,2.696138351516));
#13254=CARTESIAN_POINT('Ctrl Pts',(11.9627650599009,10.5958192942303,2.58249696621083));
#13255=CARTESIAN_POINT('Ctrl Pts',(11.7646035860733,10.4371523366744,2.46864604141759));
#13256=CARTESIAN_POINT('Ctrl Pts',(11.5611715157476,10.2742652373588,2.35176696854934));
#13257=CARTESIAN_POINT('Ctrl Pts',(11.3577645693235,10.1105684093222,2.23466749726835));
#13258=CARTESIAN_POINT('Ctrl Pts',(11.155138812055,9.94654008829857,2.11780296935806));
#13259=CARTESIAN_POINT('Ctrl Pts',(10.9369442531883,9.76990860950791,1.99195912572088));
#13260=CARTESIAN_POINT('Ctrl Pts',(10.7196555410844,9.59289262515108,1.86638826421842));
#13261=CARTESIAN_POINT('Ctrl Pts',(10.5042167520018,9.41614744679641,1.74168466284163));
#13262=CARTESIAN_POINT('Ctrl Pts',(10.3518588411108,9.29115358543629,1.6534945079152));
#13263=CARTESIAN_POINT('Ctrl Pts',(10.2004261307572,9.16629650496073,1.56573868767396));
#13264=CARTESIAN_POINT('Ctrl Pts',(10.0502525316942,9.041822881172,1.47863151154858));
#13265=CARTESIAN_POINT('Ctrl Pts',(15.8,13.5950405390087,4.75758878307678));
#13266=CARTESIAN_POINT('Ctrl Pts',(15.8,13.6029203421718,4.76123078081695));
#13267=CARTESIAN_POINT('Ctrl Pts',(15.8,13.610814146196,4.76483261634472));
#13268=CARTESIAN_POINT('Ctrl Pts',(15.8,13.6187219510797,4.76839428970851));
#13269=CARTESIAN_POINT('Ctrl Pts',(15.8,13.626643760007,4.77191579174908));
#13270=CARTESIAN_POINT('Ctrl Pts',(15.8,13.6345795785203,4.77539710335946));
#13271=CARTESIAN_POINT('Ctrl Pts',(10.0502525316942,10.5073910450885,-2.3220627978979));
#13272=CARTESIAN_POINT('Ctrl Pts',(11.1454425256572,11.7253388222013,-2.01816863800157));
#13273=CARTESIAN_POINT('Ctrl Pts',(12.3775312688656,13.0955300714531,-1.67628770811821));
#13274=CARTESIAN_POINT('Ctrl Pts',(13.7465187613193,14.617964792844,-1.29642000824781));
#13275=CARTESIAN_POINT('Ctrl Pts',(14.2941137583008,15.2269386814004,-1.14447292829965));
#13276=CARTESIAN_POINT('Ctrl Pts',(14.8417087552824,15.8359125699568,-0.992525848351485));
#13277=CARTESIAN_POINT('Ctrl Pts',(15.3208543776412,16.3687647224436,-0.859572153396845));
#13278=CARTESIAN_POINT('Ctrl Pts',(15.5946518761319,16.6732516667218,-0.783598613422764));
#13279=CARTESIAN_POINT('Ctrl Pts',(15.7315506253773,16.8254951388609,-0.745611843435724));
#13280=CARTESIAN_POINT('Ctrl Pts',(15.8,16.9016168749304,-0.726618458442204));
#13281=CARTESIAN_POINT('Ctrl Pts',(10.0502525316942,10.3973886408451,-2.57345271232945));
#13282=CARTESIAN_POINT('Ctrl Pts',(11.1454425256572,11.618687280661,-2.29815463811992));
#13283=CARTESIAN_POINT('Ctrl Pts',(12.3775312688656,12.9928273987101,-1.98887116228557));
#13284=CARTESIAN_POINT('Ctrl Pts',(13.7465187613193,14.519468077176,-1.64478997784958));
#13285=CARTESIAN_POINT('Ctrl Pts',(14.2941137583008,15.1301263986154,-1.50716238874916));
#13286=CARTESIAN_POINT('Ctrl Pts',(14.8417087552824,15.740805777741,-1.36958497392712));
#13287=CARTESIAN_POINT('Ctrl Pts',(15.3208543776412,16.2751437253593,-1.24918922664557));
#13288=CARTESIAN_POINT('Ctrl Pts',(15.5946518761319,16.5804716520035,-1.18037249165619));
#13289=CARTESIAN_POINT('Ctrl Pts',(15.7315506253773,16.7331376997671,-1.14596909077303));
#13290=CARTESIAN_POINT('Ctrl Pts',(15.8,16.8094688647556,-1.12876296113493));
#13291=CARTESIAN_POINT('Ctrl Pts',(10.0502525316942,10.189368118401,-2.93870070814821));
#13292=CARTESIAN_POINT('Ctrl Pts',(11.1454425256572,11.4106316171747,-2.70946206711306));
#13293=CARTESIAN_POINT('Ctrl Pts',(12.3775312688656,12.7843360022416,-2.45105312324518));
#13294=CARTESIAN_POINT('Ctrl Pts',(13.7465187613194,14.310894320163,-2.16445481731473));
#13295=CARTESIAN_POINT('Ctrl Pts',(14.2941137583009,14.9215151635443,-2.04980959621707));
#13296=CARTESIAN_POINT('Ctrl Pts',(14.8417087552824,15.5321104940175,-1.93510378473096));
#13297=CARTESIAN_POINT('Ctrl Pts',(15.3208543776412,16.0663892944466,-1.83475492870443));
#13298=CARTESIAN_POINT('Ctrl Pts',(15.594651876132,16.3717012113088,-1.77743586902584));
#13299=CARTESIAN_POINT('Ctrl Pts',(15.7315506253773,16.5243546442885,-1.7487703415134));
#13300=CARTESIAN_POINT('Ctrl Pts',(15.8,16.6006836129618,-1.7344429264487));
#13301=CARTESIAN_POINT('Ctrl Pts',(10.0502525316942,9.95881139224219,-3.05808383535426));
#13302=CARTESIAN_POINT('Ctrl Pts',(11.1454425256572,11.1626816238278,-2.85649631904975));
#13303=CARTESIAN_POINT('Ctrl Pts',(12.3775312688656,12.5171248305866,-2.62997738853438));
#13304=CARTESIAN_POINT('Ctrl Pts',(13.7465187613193,14.0219712727573,-2.37801889657081));
#13305=CARTESIAN_POINT('Ctrl Pts',(14.2941137583008,14.6239108703276,-2.27723855544496));
#13306=CARTESIAN_POINT('Ctrl Pts',(14.8417087552823,15.225860952321,-2.17648960137064));
#13307=CARTESIAN_POINT('Ctrl Pts',(15.3208543776412,15.7525640332375,-2.08832456454097));
#13308=CARTESIAN_POINT('Ctrl Pts',(15.5946518761319,16.0535332175881,-2.03793255455516));
#13309=CARTESIAN_POINT('Ctrl Pts',(15.7315506253773,16.2040188475872,-2.01273965647872));
#13310=CARTESIAN_POINT('Ctrl Pts',(15.8,16.2792607370613,-2.00014043670969));
#13311=CARTESIAN_POINT('Ctrl Pts',(10.0502525316942,9.78147886731912,-3.07559947603193));
#13312=CARTESIAN_POINT('Ctrl Pts',(11.1454425256572,10.9672359168267,-2.88676320881926));
#13313=CARTESIAN_POINT('Ctrl Pts',(12.3775312688656,12.3013551830101,-2.67450622091512));
#13314=CARTESIAN_POINT('Ctrl Pts',(13.7465187613193,13.7835653267336,-2.4384787180816));
#13315=CARTESIAN_POINT('Ctrl Pts',(14.2941137583008,14.3764510158762,-2.34406982037813));
#13316=CARTESIAN_POINT('Ctrl Pts',(14.8417087552824,14.9693534649946,-2.2496825286364));
#13317=CARTESIAN_POINT('Ctrl Pts',(15.3208543776412,15.4881379273167,-2.16708696976893));
#13318=CARTESIAN_POINT('Ctrl Pts',(15.5946518761319,15.7845797896778,-2.11988125471032));
#13319=CARTESIAN_POINT('Ctrl Pts',(15.7315506253773,15.9328023798814,-2.09628053589475));
#13320=CARTESIAN_POINT('Ctrl Pts',(15.8,16.0069121954757,-2.08447826919396));
#13321=CARTESIAN_POINT('Ctrl Pts',(10.0502525316942,9.60383008034201,-3.1022368453188));
#13322=CARTESIAN_POINT('Ctrl Pts',(11.1454425256572,10.7718807970721,-2.92542368552957));
#13323=CARTESIAN_POINT('Ctrl Pts',(12.3775312688656,12.0859609655105,-2.72674232124834));
#13324=CARTESIAN_POINT('Ctrl Pts',(13.7465187613193,13.5460266034681,-2.50574851695231));
#13325=CARTESIAN_POINT('Ctrl Pts',(14.2941137583008,14.1300531231308,-2.41735366657092));
#13326=CARTESIAN_POINT('Ctrl Pts',(14.8417087552823,14.7140823594691,-2.3289862555658));
#13327=CARTESIAN_POINT('Ctrl Pts',(15.3208543776412,15.2251071015168,-2.25165628918294));
#13328=CARTESIAN_POINT('Ctrl Pts',(15.5946518761319,15.5171202021386,-2.20745725592095));
#13329=CARTESIAN_POINT('Ctrl Pts',(15.7315506253773,15.6631270213657,-2.18536045543709));
#13330=CARTESIAN_POINT('Ctrl Pts',(15.8,15.7361301911613,-2.17430963295026));
#13331=CARTESIAN_POINT('Ctrl Pts',(10.0502525316942,9.33616641898042,-3.16416975479848));
#13332=CARTESIAN_POINT('Ctrl Pts',(11.1454425256572,10.4789053528453,-3.00789330574876));
#13333=CARTESIAN_POINT('Ctrl Pts',(12.3775312688656,11.7645911992084,-2.83212323706007));
#13334=CARTESIAN_POINT('Ctrl Pts',(13.7465187613193,13.1930250082462,-2.6367816468882));
#13335=CARTESIAN_POINT('Ctrl Pts',(14.2941137583008,13.7643997282132,-2.55864547926933));
#13336=CARTESIAN_POINT('Ctrl Pts',(14.8417087552823,14.3357867368398,-2.48051412346291));
#13337=CARTESIAN_POINT('Ctrl Pts',(15.3208543776412,14.8357465708549,-2.4121476997586));
#13338=CARTESIAN_POINT('Ctrl Pts',(15.5946518761319,15.1214332106675,-2.37307933395525));
#13339=CARTESIAN_POINT('Ctrl Pts',(15.7315506253773,15.2642777469938,-2.35354562736143));
#13340=CARTESIAN_POINT('Ctrl Pts',(15.8,15.3356989303604,-2.34377834929582));
#13341=CARTESIAN_POINT('Ctrl Pts',(10.0502525316942,9.08015411140624,-3.1498793996228));
#13342=CARTESIAN_POINT('Ctrl Pts',(11.1454425256572,10.19428901683,-3.0067293155267));
#13343=CARTESIAN_POINT('Ctrl Pts',(12.3775312688656,11.4477380681646,-2.84574388114627));
#13344=CARTESIAN_POINT('Ctrl Pts',(13.7465187613193,12.8404112867165,-2.66681194224705));
#13345=CARTESIAN_POINT('Ctrl Pts',(14.2941137583008,13.3974811152093,-2.59523983509502));
#13346=CARTESIAN_POINT('Ctrl Pts',(14.8417087552823,13.9545565014729,-2.52367459367682));
#13347=CARTESIAN_POINT('Ctrl Pts',(15.3208543776412,14.4419957464975,-2.46105288517697));
#13348=CARTESIAN_POINT('Ctrl Pts',(15.5946518761319,14.7205303350335,-2.42526642923796));
#13349=CARTESIAN_POINT('Ctrl Pts',(15.7315506253773,14.8597981794496,-2.40737388088826));
#13350=CARTESIAN_POINT('Ctrl Pts',(15.8,14.9294316110386,-2.39842700063225));
#13351=CARTESIAN_POINT('Ctrl Pts',(10.0502525316942,8.83780343943476,-3.10442465522081));
#13352=CARTESIAN_POINT('Ctrl Pts',(11.1454425256572,9.9230791616099,-2.96904269314958));
#13353=CARTESIAN_POINT('Ctrl Pts',(12.3775312688656,11.1440266947135,-2.81681208487056));
#13354=CARTESIAN_POINT('Ctrl Pts',(13.7465187613194,12.5006225450517,-2.64759182043347));
#13355=CARTESIAN_POINT('Ctrl Pts',(14.2941137583009,13.0432610264625,-2.57990456259871));
#13356=CARTESIAN_POINT('Ctrl Pts',(14.8417087552824,13.585900959023,-2.51222601461465));
#13357=CARTESIAN_POINT('Ctrl Pts',(15.3208543776412,14.0607104514503,-2.45300459283688));
#13358=CARTESIAN_POINT('Ctrl Pts',(15.594651876132,14.3320296071118,-2.41916045348294));
#13359=CARTESIAN_POINT('Ctrl Pts',(15.7315506253773,14.4676893285878,-2.40223924596973));
#13360=CARTESIAN_POINT('Ctrl Pts',(15.8,14.5355190612237,-2.39377787334028));
#13361=CARTESIAN_POINT('Ctrl Pts',(10.0502525316942,8.72224646189196,-3.06201554081689));
#13362=CARTESIAN_POINT('Ctrl Pts',(11.1454425256572,9.79262845293104,-2.92828468444751));
#13363=CARTESIAN_POINT('Ctrl Pts',(12.3775312688656,10.9969124481398,-2.77780914227504));
#13364=CARTESIAN_POINT('Ctrl Pts',(13.7465187613193,12.3349000504671,-2.61064282371592));
#13365=CARTESIAN_POINT('Ctrl Pts',(14.2941137583008,12.870096284426,-2.54377597211689));
#13366=CARTESIAN_POINT('Ctrl Pts',(14.8417087552824,13.4053047729009,-2.47690579066087));
#13367=CARTESIAN_POINT('Ctrl Pts',(15.3208543776412,13.8736084123374,-2.41839541117504));
#13368=CARTESIAN_POINT('Ctrl Pts',(15.5946518761319,14.1412058111469,-2.38496218052017));
#13369=CARTESIAN_POINT('Ctrl Pts',(15.7315506253773,14.2750057235919,-2.3682452355795));
#13370=CARTESIAN_POINT('Ctrl Pts',(15.8,14.3419045980318,-2.35988705705642));
#13371=CARTESIAN_POINT('Ctrl Pts',(10.0502525316942,8.64769560732005,-3.02626384252387));
#13372=CARTESIAN_POINT('Ctrl Pts',(11.1454425256572,9.70806748165927,-2.89260526381667));
#13373=CARTESIAN_POINT('Ctrl Pts',(12.3775312688656,10.9009858402909,-2.74223936277106));
#13374=CARTESIAN_POINT('Ctrl Pts',(13.7465187613193,12.2264506832149,-2.57516613938705));
#13375=CARTESIAN_POINT('Ctrl Pts',(14.2941137583008,12.7566366203845,-2.50833685003344));
#13376=CARTESIAN_POINT('Ctrl Pts',(14.8417087552824,13.2868225575541,-2.44150756067984));
#13377=CARTESIAN_POINT('Ctrl Pts',(15.3208543776412,13.7507352525775,-2.38303193249544));
#13378=CARTESIAN_POINT('Ctrl Pts',(15.5946518761319,14.0158282211623,-2.34961728781863));
#13379=CARTESIAN_POINT('Ctrl Pts',(15.7315506253773,14.1483747054547,-2.33290996548023));
#13380=CARTESIAN_POINT('Ctrl Pts',(15.8,14.2146479476009,-2.32455630431103));
#13381=CARTESIAN_POINT('',(15.8,14.2146479476009,-2.32455630431103));
#13382=CARTESIAN_POINT('Ctrl Pts',(15.8,14.2566004799664,-2.33570557485288));
#13383=CARTESIAN_POINT('Ctrl Pts',(15.8,14.2481979205348,-2.33357202566326));
#13384=CARTESIAN_POINT('Ctrl Pts',(15.8,14.2398013892846,-2.33139031275994));
#13385=CARTESIAN_POINT('Ctrl Pts',(15.8,14.2314108839843,-2.32916045010432));
#13386=CARTESIAN_POINT('Ctrl Pts',(15.8,14.2230264034132,-2.326882447186));
#13387=CARTESIAN_POINT('Ctrl Pts',(15.8,14.2146479476009,-2.32455630431103));
#13388=CARTESIAN_POINT('Ctrl Pts',(10.0502525316942,8.64769560732005,-3.02626384252387));
#13389=CARTESIAN_POINT('Ctrl Pts',(10.2399538592853,8.8379156589892,-3.00625338967613));
#13390=CARTESIAN_POINT('Ctrl Pts',(10.4321310528899,9.02976542249266,-2.98528677263247));
#13391=CARTESIAN_POINT('Ctrl Pts',(10.6260535771571,9.2224931401807,-2.96359080496244));
#13392=CARTESIAN_POINT('Ctrl Pts',(10.8154434277103,9.41071611112395,-2.9424019508561));
#13393=CARTESIAN_POINT('Ctrl Pts',(11.0064979730134,9.59977633037444,-2.92051732350852));
#13394=CARTESIAN_POINT('Ctrl Pts',(11.1985367155046,9.78902046263136,-2.89813133617984));
#13395=CARTESIAN_POINT('Ctrl Pts',(11.389602998892,9.97730628732557,-2.87585870856646));
#13396=CARTESIAN_POINT('Ctrl Pts',(11.581643537013,10.1657740234639,-2.85308955972937));
#13397=CARTESIAN_POINT('Ctrl Pts',(11.7739881178967,10.3538294697525,-2.83000106681659));
#13398=CARTESIAN_POINT('Ctrl Pts',(11.9659332365647,10.5414943615222,-2.80696052420475));
#13399=CARTESIAN_POINT('Ctrl Pts',(12.1581811364316,10.7287485903511,-2.78360167031422));
#13400=CARTESIAN_POINT('Ctrl Pts',(12.3500657725596,10.9150525380988,-2.76009024231676));
#13401=CARTESIAN_POINT('Ctrl Pts',(12.5349538836681,11.0945634446842,-2.73743609136633));
#13402=CARTESIAN_POINT('Ctrl Pts',(12.7195047388315,11.2731923646039,-2.7146399954872));
#13403=CARTESIAN_POINT('Ctrl Pts',(12.9031225251803,11.4505020946774,-2.69184501333336));
#13404=CARTESIAN_POINT('Ctrl Pts',(13.0466099992771,11.5890601603578,-2.67403195460754));
#13405=CARTESIAN_POINT('Ctrl Pts',(13.1909144693232,11.7281274609627,-2.65603885317597));
#13406=CARTESIAN_POINT('Ctrl Pts',(13.3358225135832,11.8675036836248,-2.63790201856914));
#13407=CARTESIAN_POINT('Ctrl Pts',(13.4722456635829,11.9987189203477,-2.6208271617472));
#13408=CARTESIAN_POINT('Ctrl Pts',(13.6092037742271,12.1302080042448,-2.60362489076148));
#13409=CARTESIAN_POINT('Ctrl Pts',(13.7465187613193,12.2618085151784,-2.58632488288814));
#13410=CARTESIAN_POINT('Ctrl Pts',(13.8831227642785,12.3927276301685,-2.56911445031434));
#13411=CARTESIAN_POINT('Ctrl Pts',(14.0200799576114,12.5237570157981,-2.55180727580019));
#13412=CARTESIAN_POINT('Ctrl Pts',(14.1572150090555,12.6547407331994,-2.53443232271127));
#13413=CARTESIAN_POINT('Ctrl Pts',(14.4088349682216,12.8950740198163,-2.50255218017504));
#13414=CARTESIAN_POINT('Ctrl Pts',(14.6610537068599,13.135250418528,-2.47044377568183));
#13415=CARTESIAN_POINT('Ctrl Pts',(14.912788167059,13.3743428798829,-2.43828616201197));
#13416=CARTESIAN_POINT('Ctrl Pts',(14.9347318651883,13.3951845747101,-2.43548298215979));
#13417=CARTESIAN_POINT('Ctrl Pts',(14.9566718834733,13.4160180659858,-2.43267942911461));
#13418=CARTESIAN_POINT('Ctrl Pts',(14.9786075045277,13.4368427586266,-2.42987562206087));
#13419=CARTESIAN_POINT('Ctrl Pts',(15.1157365203996,13.5670268824575,-2.4123478164419));
#13420=CARTESIAN_POINT('Ctrl Pts',(15.252693690801,13.6968667539964,-2.39481006097156));
#13421=CARTESIAN_POINT('Ctrl Pts',(15.3893037522639,13.8262197421006,-2.37729164508551));
#13422=CARTESIAN_POINT('Ctrl Pts',(15.4578478923357,13.8911226433977,-2.368501774563));
#13423=CARTESIAN_POINT('Ctrl Pts',(15.5263046465628,13.9559030572658,-2.35971677469616));
#13424=CARTESIAN_POINT('Ctrl Pts',(15.5946518761319,14.0205434363407,-2.35094037726561));
#13425=CARTESIAN_POINT('Ctrl Pts',(15.663218932117,14.085391719422,-2.34213575215115));
#13426=CARTESIAN_POINT('Ctrl Pts',(15.7316757577788,14.1500990399651,-2.33333979124571));
#13427=CARTESIAN_POINT('Ctrl Pts',(15.8,14.2146479476009,-2.32455630431103));
#13428=CARTESIAN_POINT('Origin',(15.8,15.0204902775358,-1.08357274193521));
#13429=CARTESIAN_POINT('Origin',(15.8,0.,0.));
#13430=CARTESIAN_POINT('Origin',(13.3251262658471,0.,0.));
#13431=CARTESIAN_POINT('',(15.8,-14.4034641071566,-1.76391562154631E-15));
#13432=CARTESIAN_POINT('',(13.3251262658471,-12.1473403730037,-1.48762015059523E-15));
#13433=CARTESIAN_POINT('Origin',(15.8,0.,0.));
#13434=CARTESIAN_POINT('',(15.8,-14.2372609598209,-2.18178336415567));
#13435=CARTESIAN_POINT('Ctrl Pts',(10.5501326772895,-9.61762388247333,-4.38386896228771E-10));
#13436=CARTESIAN_POINT('Ctrl Pts',(11.3205407897314,-10.3199368948271,-0.318347952011169));
#13437=CARTESIAN_POINT('Ctrl Pts',(12.1203771071554,-11.0330476815418,-0.652342287974112));
#13438=CARTESIAN_POINT('Ctrl Pts',(13.8535773385734,-12.5583034272282,-1.37415173034123));
#13439=CARTESIAN_POINT('Ctrl Pts',(14.8398793216181,-13.4127296512147,-1.78409574717497));
#13440=CARTESIAN_POINT('Ctrl Pts',(15.8,-14.2372609598209,-2.18178336415567));
#13441=CARTESIAN_POINT('Origin',(15.8,0.,0.));
#13442=CARTESIAN_POINT('',(15.8,-12.8662316724636,-6.47455487556025));
#13443=CARTESIAN_POINT('Ctrl Pts',(10.0502525316942,-8.77492596468499,-2.63468906623289));
#13444=CARTESIAN_POINT('Ctrl Pts',(10.2391461906127,-8.9164502426962,-2.76214144474561));
#13445=CARTESIAN_POINT('Ctrl Pts',(10.4304946780272,-9.05872439496926,-2.89131047500302));
#13446=CARTESIAN_POINT('Ctrl Pts',(10.6235767498548,-9.20127947078457,-3.02157840065359));
#13447=CARTESIAN_POINT('Ctrl Pts',(10.8128907594447,-9.34105253585759,-3.14930410347228));
#13448=CARTESIAN_POINT('Ctrl Pts',(11.003871350703,-9.48109547783796,-3.27808626456685));
#13449=CARTESIAN_POINT('Ctrl Pts',(11.1958386868234,-9.6209944304455,-3.40738413972936));
#13450=CARTESIAN_POINT('Ctrl Pts',(11.3869496174041,-9.76026926521909,-3.53610519063208));
#13451=CARTESIAN_POINT('Ctrl Pts',(11.5790385083443,-9.89940114828137,-3.66533747024572));
#13452=CARTESIAN_POINT('Ctrl Pts',(11.7714345809798,-10.0380132338096,-3.79458803732579));
#13453=CARTESIAN_POINT('Ctrl Pts',(11.963522415819,-10.1764032488808,-3.92363153203988));
#13454=CARTESIAN_POINT('Ctrl Pts',(12.1559164488704,-10.3142748929476,-4.05269344373601));
#13455=CARTESIAN_POINT('Ctrl Pts',(12.3479491202715,-10.4512882521924,-4.18132152636412));
#13456=CARTESIAN_POINT('Ctrl Pts',(12.5335453523396,-10.5837092773923,-4.30563832776951));
#13457=CARTESIAN_POINT('Ctrl Pts',(12.7188040406165,-10.7153286091805,-4.42955027592032));
#13458=CARTESIAN_POINT('Ctrl Pts',(12.9031225251803,-10.8458735001829,-4.55268038845334));
#13459=CARTESIAN_POINT('Ctrl Pts',(13.1554739610253,-11.0246032177402,-4.72125849263535));
#13460=CARTESIAN_POINT('Ctrl Pts',(13.4103523866339,-11.2042784469548,-4.89121179563063));
#13461=CARTESIAN_POINT('Ctrl Pts',(13.6665968506683,-11.3841414734476,-5.06174747048486));
#13462=CARTESIAN_POINT('Ctrl Pts',(13.9194672603243,-11.5616361848461,-5.2300376465239));
#13463=CARTESIAN_POINT('Ctrl Pts',(14.1736679711014,-11.7393134647369,-5.39889509460765));
#13464=CARTESIAN_POINT('Ctrl Pts',(14.428083290334,-11.9164831860886,-5.56759036901415));
#13465=CARTESIAN_POINT('Ctrl Pts',(14.6797373390534,-12.0917300140828,-5.73445472660187));
#13466=CARTESIAN_POINT('Ctrl Pts',(14.9316013630469,-12.2664800265877,-5.9011605955206));
#13467=CARTESIAN_POINT('Ctrl Pts',(15.1825956039693,-12.4401067548811,-6.06703163029926));
#13468=CARTESIAN_POINT('Ctrl Pts',(15.3891870324172,-12.5830175789824,-6.2035588027441));
#13469=CARTESIAN_POINT('Ctrl Pts',(15.5951891994095,-12.7251681216495,-6.3395209766308));
#13470=CARTESIAN_POINT('Ctrl Pts',(15.8,-12.8662316724636,-6.47455487556025));
#13471=CARTESIAN_POINT('Origin',(15.8,0.,0.));
#13472=CARTESIAN_POINT('',(15.8,-10.2357659846983,-10.1335518448686));
#13473=CARTESIAN_POINT('Ctrl Pts',(10.0502525316942,-7.53128682236137,-5.21733945232202));
#13474=CARTESIAN_POINT('Ctrl Pts',(10.2399700857352,-7.62691474601356,-5.38300672530998));
#13475=CARTESIAN_POINT('Ctrl Pts',(10.4321639293634,-7.72272706183512,-5.55055481152833));
#13476=CARTESIAN_POINT('Ctrl Pts',(10.6261033397486,-7.81846533797986,-5.71924202232276));
#13477=CARTESIAN_POINT('Ctrl Pts',(10.815494732925,-7.9119584834078,-5.88397339796183));
#13478=CARTESIAN_POINT('Ctrl Pts',(11.0065507832424,-8.00538083967114,-6.04979105175822));
#13479=CARTESIAN_POINT('Ctrl Pts',(11.1985909796536,-8.09850566734927,-6.21605213671099));
#13480=CARTESIAN_POINT('Ctrl Pts',(11.3896566244814,-8.19115791194337,-6.38146949203504));
#13481=CARTESIAN_POINT('Ctrl Pts',(11.5816964522019,-8.28351537255339,-6.54732580586895));
#13482=CARTESIAN_POINT('Ctrl Pts',(11.774040259505,-8.37537212829127,-6.71303622283048));
#13483=CARTESIAN_POINT('Ctrl Pts',(11.9659830376821,-8.46703736637656,-6.87840114021702));
#13484=CARTESIAN_POINT('Ctrl Pts',(12.1582285291929,-8.55820369955463,-7.04362087245224));
#13485=CARTESIAN_POINT('Ctrl Pts',(12.350110714034,-8.64868803888439,-7.20816146064353));
#13486=CARTESIAN_POINT('Ctrl Pts',(12.5349837899972,-8.73586714908811,-7.36669167899034));
#13487=CARTESIAN_POINT('Ctrl Pts',(12.7195196163976,-8.82241309395645,-7.52459184596087));
#13488=CARTESIAN_POINT('Ctrl Pts',(12.9031225251803,-8.90818466253794,-7.68142427504574));
#13489=CARTESIAN_POINT('Ctrl Pts',(13.0466099992771,-8.97521598468134,-7.80399035667839));
#13490=CARTESIAN_POINT('Ctrl Pts',(13.1909144693232,-9.04240096834747,-7.92707423833476));
#13491=CARTESIAN_POINT('Ctrl Pts',(13.3358225135832,-9.10965124727546,-8.05049252087456));
#13492=CARTESIAN_POINT('Ctrl Pts',(13.4722456635829,-9.17296377720826,-8.16668421304467));
#13493=CARTESIAN_POINT('Ctrl Pts',(13.6092037742271,-9.23633418862365,-8.28317233887351));
#13494=CARTESIAN_POINT('Ctrl Pts',(13.7465187613193,-9.29969102606761,-8.39980806233602));
#13495=CARTESIAN_POINT('Ctrl Pts',(13.8831227642785,-9.36271981697347,-8.51583987394238));
#13496=CARTESIAN_POINT('Ctrl Pts',(14.0200799576114,-9.42573515876482,-8.63201776215884));
#13497=CARTESIAN_POINT('Ctrl Pts',(14.1572150090555,-9.48866882093701,-8.74819853760654));
#13498=CARTESIAN_POINT('Ctrl Pts',(14.4088743845442,-9.60415968890035,-8.96140428686672));
#13499=CARTESIAN_POINT('Ctrl Pts',(14.6611327271176,-9.71937357878302,-9.17461726586999));
#13500=CARTESIAN_POINT('Ctrl Pts',(14.9129064698008,-9.83391026822831,-9.38698186590304));
#13501=CARTESIAN_POINT('Ctrl Pts',(14.9348107204665,-9.84387493066409,-9.40545753132419));
#13502=CARTESIAN_POINT('Ctrl Pts',(14.9567113032174,-9.85383448723409,-9.42392680146211));
#13503=CARTESIAN_POINT('Ctrl Pts',(14.9786075045277,-9.86378868594609,-9.44238912780876));
#13504=CARTESIAN_POINT('Ctrl Pts',(15.1157365203996,-9.92612869889287,-9.55801286576867));
#13505=CARTESIAN_POINT('Ctrl Pts',(15.252693690801,-9.98825831748494,-9.67336395156665));
#13506=CARTESIAN_POINT('Ctrl Pts',(15.3893037522639,-10.0501174002428,-9.78830977806043));
#13507=CARTESIAN_POINT('Ctrl Pts',(15.4578478923357,-10.0811552139138,-9.84598388161831));
#13508=CARTESIAN_POINT('Ctrl Pts',(15.5263046465628,-10.1121249718658,-9.90355602888934));
#13509=CARTESIAN_POINT('Ctrl Pts',(15.5946518761319,-10.1430193787867,-9.96100982960575));
#13510=CARTESIAN_POINT('Ctrl Pts',(15.663218932117,-10.1740131519407,-10.0186484200082));
#13511=CARTESIAN_POINT('Ctrl Pts',(15.7316757577788,-10.2049310789385,-10.076167877539));
#13512=CARTESIAN_POINT('Ctrl Pts',(15.8,-10.2357659846983,-10.1335518448686));
#13513=CARTESIAN_POINT('Origin',(15.8,0.,0.));
#13514=CARTESIAN_POINT('',(15.8,-6.60335220557564,-12.8006061549939));
#13515=CARTESIAN_POINT('Ctrl Pts',(10.0502525316942,-5.55043285230422,-7.28928030147641));
#13516=CARTESIAN_POINT('Ctrl Pts',(10.2399762236023,-5.5901876956016,-7.4763959480264));
#13517=CARTESIAN_POINT('Ctrl Pts',(10.4321763653293,-5.62953666502947,-7.66535745978647));
#13518=CARTESIAN_POINT('Ctrl Pts',(10.6261221631202,-5.66846318065116,-7.85537951329684));
#13519=CARTESIAN_POINT('Ctrl Pts',(10.8155134734716,-5.70647557321124,-8.04093922183353));
#13520=CARTESIAN_POINT('Ctrl Pts',(11.0065694150242,-5.74408496164277,-8.22751014665864));
#13521=CARTESIAN_POINT('Ctrl Pts',(11.1986094788125,-5.78127435838156,-8.41441083753434));
#13522=CARTESIAN_POINT('Ctrl Pts',(11.389674403306,-5.81827491513876,-8.60036248577636));
#13523=CARTESIAN_POINT('Ctrl Pts',(11.5817134810757,-5.85485947501131,-8.78664049259207));
#13524=CARTESIAN_POINT('Ctrl Pts',(11.7740565170535,-5.89101292727639,-8.97262500016449));
#13525=CARTESIAN_POINT('Ctrl Pts',(11.9659982062668,-5.92709094103641,-9.15822142880287));
#13526=CARTESIAN_POINT('Ctrl Pts',(12.1582425865211,-5.96273934048993,-9.34352559234182));
#13527=CARTESIAN_POINT('Ctrl Pts',(12.350123649327,-5.9979490001613,-9.5279730968269));
#13528=CARTESIAN_POINT('Ctrl Pts',(12.5349923977945,-6.03187191898524,-9.70567994717204));
#13529=CARTESIAN_POINT('Ctrl Pts',(12.7195238985382,-6.06538737998552,-9.88259194572981));
#13530=CARTESIAN_POINT('Ctrl Pts',(12.9031225251803,-6.0984963351851,-10.0582492231335));
#13531=CARTESIAN_POINT('Ctrl Pts',(13.0466099992771,-6.12437191191712,-10.1955303101566));
#13532=CARTESIAN_POINT('Ctrl Pts',(13.1909144693232,-6.15023362158894,-10.3333513349338));
#13533=CARTESIAN_POINT('Ctrl Pts',(13.3358225135832,-6.17605409599263,-10.4715105676525));
#13534=CARTESIAN_POINT('Ctrl Pts',(13.4722456635829,-6.20036268749026,-10.6015800736297));
#13535=CARTESIAN_POINT('Ctrl Pts',(13.6092037742271,-6.22463472522239,-10.7319493881454));
#13536=CARTESIAN_POINT('Ctrl Pts',(13.7465187613193,-6.24884824365307,-10.8624548834565));
#13537=CARTESIAN_POINT('Ctrl Pts',(13.8831227642785,-6.27293639028148,-10.9922846525529));
#13538=CARTESIAN_POINT('Ctrl Pts',(14.0200799576114,-6.29696660630782,-11.1222491940658));
#13539=CARTESIAN_POINT('Ctrl Pts',(14.1572150090555,-6.32091824773854,-11.2521912379382));
#13540=CARTESIAN_POINT('Ctrl Pts',(14.4088957070015,-6.36487612552952,-11.4906707801847));
#13541=CARTESIAN_POINT('Ctrl Pts',(14.6611754735345,-6.40856830116458,-11.7290715847991));
#13542=CARTESIAN_POINT('Ctrl Pts',(14.9129704662325,-6.45187850892463,-11.9664560266787));
#13543=CARTESIAN_POINT('Ctrl Pts',(14.9348533776129,-6.45564249735079,-11.987086550936));
#13544=CARTESIAN_POINT('Ctrl Pts',(14.9567326275257,-6.45940361158542,-12.0077094295138));
#13545=CARTESIAN_POINT('Ctrl Pts',(14.9786075045277,-6.46316178167156,-12.0283240646364));
#13546=CARTESIAN_POINT('Ctrl Pts',(15.1157365203996,-6.48672096169998,-12.1575528884896));
#13547=CARTESIAN_POINT('Ctrl Pts',(15.252693690801,-6.5101642983752,-12.2864573923713));
#13548=CARTESIAN_POINT('Ctrl Pts',(15.3893037522639,-6.53347557107031,-12.4148928744451));
#13549=CARTESIAN_POINT('Ctrl Pts',(15.4578478923357,-6.54517200926641,-12.4793354168112));
#13550=CARTESIAN_POINT('Ctrl Pts',(15.5263046465628,-6.5568352285584,-12.5436599631772));
#13551=CARTESIAN_POINT('Ctrl Pts',(15.5946518761319,-6.56846335549623,-12.6078486707221));
#13552=CARTESIAN_POINT('Ctrl Pts',(15.663218932117,-6.58012888218654,-12.6722438295541));
#13553=CARTESIAN_POINT('Ctrl Pts',(15.7316757577788,-6.59175908863286,-12.7365022490344));
#13554=CARTESIAN_POINT('Ctrl Pts',(15.8,-6.60335220557564,-12.8006061549939));
#13555=CARTESIAN_POINT('Origin',(15.8,0.,0.));
#13556=CARTESIAN_POINT('',(15.8,-2.32455630431103,-14.2146479476009));
#13557=CARTESIAN_POINT('Ctrl Pts',(10.0502525316942,-3.02626384252387,-8.64769560732005));
#13558=CARTESIAN_POINT('Ctrl Pts',(10.239953859285,-3.00625338967615,-8.83791565898895));
#13559=CARTESIAN_POINT('Ctrl Pts',(10.4321310528894,-2.98528677263252,-9.02976542249216));
#13560=CARTESIAN_POINT('Ctrl Pts',(10.6260535771564,-2.96359080496253,-9.22249314017995));
#13561=CARTESIAN_POINT('Ctrl Pts',(10.8154434277096,-2.94240195085618,-9.41071611112327));
#13562=CARTESIAN_POINT('Ctrl Pts',(11.0064979730128,-2.92051732350859,-9.59977633037382));
#13563=CARTESIAN_POINT('Ctrl Pts',(11.1985367155041,-2.8981313361799,-9.78902046263081));
#13564=CARTESIAN_POINT('Ctrl Pts',(11.3896029988914,-2.87585870856653,-9.97730628732503));
#13565=CARTESIAN_POINT('Ctrl Pts',(11.5816435370124,-2.85308955972943,-10.1657740234633));
#13566=CARTESIAN_POINT('Ctrl Pts',(11.7739881178962,-2.83000106681665,-10.353829469752));
#13567=CARTESIAN_POINT('Ctrl Pts',(11.9659332365641,-2.80696052420482,-10.5414943615216));
#13568=CARTESIAN_POINT('Ctrl Pts',(12.158181136431,-2.7836016703143,-10.7287485903505));
#13569=CARTESIAN_POINT('Ctrl Pts',(12.350065772559,-2.76009024231684,-10.9150525380982));
#13570=CARTESIAN_POINT('Ctrl Pts',(12.5349538836676,-2.73743609136638,-11.0945634446838));
#13571=CARTESIAN_POINT('Ctrl Pts',(12.7195047388313,-2.71463999548723,-11.2731923646037));
#13572=CARTESIAN_POINT('Ctrl Pts',(12.9031225251803,-2.69184501333336,-11.4505020946774));
#13573=CARTESIAN_POINT('Ctrl Pts',(13.0466099992771,-2.67403195460754,-11.5890601603578));
#13574=CARTESIAN_POINT('Ctrl Pts',(13.1909144693232,-2.65603885317597,-11.7281274609627));
#13575=CARTESIAN_POINT('Ctrl Pts',(13.3358225135832,-2.63790201856914,-11.8675036836248));
#13576=CARTESIAN_POINT('Ctrl Pts',(13.4722456635829,-2.6208271617472,-11.9987189203477));
#13577=CARTESIAN_POINT('Ctrl Pts',(13.6092037742271,-2.60362489076148,-12.1302080042448));
#13578=CARTESIAN_POINT('Ctrl Pts',(13.7465187613193,-2.58632488288814,-12.2618085151784));
#13579=CARTESIAN_POINT('Ctrl Pts',(13.8831227642785,-2.56911445031434,-12.3927276301685));
#13580=CARTESIAN_POINT('Ctrl Pts',(14.0200799576114,-2.55180727580019,-12.5237570157982));
#13581=CARTESIAN_POINT('Ctrl Pts',(14.1572150090555,-2.53443232271127,-12.6547407331994));
#13582=CARTESIAN_POINT('Ctrl Pts',(14.4088349682216,-2.50255218017505,-12.8950740198162));
#13583=CARTESIAN_POINT('Ctrl Pts',(14.6610537068598,-2.47044377568185,-13.1352504185278));
#13584=CARTESIAN_POINT('Ctrl Pts',(14.9127881670588,-2.438286162012,-13.3743428798827));
#13585=CARTESIAN_POINT('Ctrl Pts',(14.9347318651881,-2.43548298215981,-13.3951845747099));
#13586=CARTESIAN_POINT('Ctrl Pts',(14.9566718834732,-2.43267942911462,-13.4160180659858));
#13587=CARTESIAN_POINT('Ctrl Pts',(14.9786075045277,-2.42987562206087,-13.4368427586266));
#13588=CARTESIAN_POINT('Ctrl Pts',(15.1157365203996,-2.4123478164419,-13.5670268824575));
#13589=CARTESIAN_POINT('Ctrl Pts',(15.252693690801,-2.39481006097156,-13.6968667539964));
#13590=CARTESIAN_POINT('Ctrl Pts',(15.3893037522639,-2.3772916450855,-13.8262197421006));
#13591=CARTESIAN_POINT('Ctrl Pts',(15.4578478923357,-2.368501774563,-13.8911226433977));
#13592=CARTESIAN_POINT('Ctrl Pts',(15.5263046465628,-2.35971677469615,-13.9559030572658));
#13593=CARTESIAN_POINT('Ctrl Pts',(15.5946518761319,-2.3509403772656,-14.0205434363407));
#13594=CARTESIAN_POINT('Ctrl Pts',(15.663218932117,-2.34213575215115,-14.085391719422));
#13595=CARTESIAN_POINT('Ctrl Pts',(15.7316757577788,-2.33333979124571,-14.1500990399651));
#13596=CARTESIAN_POINT('Ctrl Pts',(15.8,-2.32455630431103,-14.2146479476009));
#13597=CARTESIAN_POINT('Origin',(15.8,0.,0.));
#13598=CARTESIAN_POINT('',(15.8,2.18178336415567,-14.2372609598209));
#13599=CARTESIAN_POINT('Ctrl Pts',(10.0502525316942,-0.205863042617262,
-9.15961421508102));
#13600=CARTESIAN_POINT('Ctrl Pts',(10.2391570234258,-0.128377591099423,
-9.33360673051062));
#13601=CARTESIAN_POINT('Ctrl Pts',(10.4305166252241,-0.0494911083977407,
-9.50884304477973));
#13602=CARTESIAN_POINT('Ctrl Pts',(10.6236099689118,0.0303537569978826,
-9.68468614630344));
#13603=CARTESIAN_POINT('Ctrl Pts',(10.8129280637648,0.108637541989126,-9.85709126570177));
#13604=CARTESIAN_POINT('Ctrl Pts',(11.0039127690162,0.187842691359046,-10.0300795089051));
#13605=CARTESIAN_POINT('Ctrl Pts',(11.195884205948,0.267582809353851,-10.2030901320277));
#13606=CARTESIAN_POINT('Ctrl Pts',(11.386997148711,0.346966330412115,-10.3753270535337));
#13607=CARTESIAN_POINT('Ctrl Pts',(11.5790880175811,0.426880221764407,-10.5475859558082));
#13608=CARTESIAN_POINT('Ctrl Pts',(11.7714860143417,0.506972115618924,-10.7193560970323));
#13609=CARTESIAN_POINT('Ctrl Pts',(11.9635738218519,0.586934883157499,-10.8908493057922));
#13610=CARTESIAN_POINT('Ctrl Pts',(12.1559677677311,0.667075331863647,-11.0618551603491));
#13611=CARTESIAN_POINT('Ctrl Pts',(12.3480002929715,0.747068390651276,-11.2319106356083));
#13612=CARTESIAN_POINT('Ctrl Pts',(12.5335794054255,0.824373216142153,-11.3962512551311));
#13613=CARTESIAN_POINT('Ctrl Pts',(12.7188209807522,0.901540748122806,-11.5597044367662));
#13614=CARTESIAN_POINT('Ctrl Pts',(12.9031225251803,0.978296811887799,-11.7218943942307));
#13615=CARTESIAN_POINT('Ctrl Pts',(13.1554719876675,1.08339279192334,-11.9439682173992));
#13616=CARTESIAN_POINT('Ctrl Pts',(13.410348400397,1.18950448019878,-12.1673662092161));
#13617=CARTESIAN_POINT('Ctrl Pts',(13.6665908392661,1.2961120061965,-12.3911227672762));
#13618=CARTESIAN_POINT('Ctrl Pts',(13.9194596713273,1.40131597126551,-12.6119334173481));
#13619=CARTESIAN_POINT('Ctrl Pts',(14.1736587969735,1.50700303047563,-12.8330929959809));
#13620=CARTESIAN_POINT('Ctrl Pts',(14.4280725441416,1.61269270111681,-13.0537197620231));
#13621=CARTESIAN_POINT('Ctrl Pts',(14.6797279548941,1.71723649159025,-13.2719545077841));
#13622=CARTESIAN_POINT('Ctrl Pts',(14.931593358573,1.82178307810192,-13.4896677845277));
#13623=CARTESIAN_POINT('Ctrl Pts',(15.1825889792242,1.92588279207063,-13.7060547738726));
#13624=CARTESIAN_POINT('Ctrl Pts',(15.3891826285177,2.01156691573547,-13.8841621753979));
#13625=CARTESIAN_POINT('Ctrl Pts',(15.5951870101943,2.09694862236073,-14.0613719009699));
#13626=CARTESIAN_POINT('Ctrl Pts',(15.8,2.18178336415567,-14.2372609598209));
#13627=CARTESIAN_POINT('Origin',(15.8,0.,0.));
#13628=CARTESIAN_POINT('',(15.8,6.47455487556025,-12.8662316724636));
#13629=CARTESIAN_POINT('Ctrl Pts',(10.0502525316942,2.63468906623289,-8.77492596468499));
#13630=CARTESIAN_POINT('Ctrl Pts',(10.2391461906127,2.76214144474559,-8.91645024269617));
#13631=CARTESIAN_POINT('Ctrl Pts',(10.4304946780271,2.89131047500297,-9.05872439496921));
#13632=CARTESIAN_POINT('Ctrl Pts',(10.6235767498547,3.02157840065351,-9.20127947078449));
#13633=CARTESIAN_POINT('Ctrl Pts',(10.8128907594447,3.1493041034723,-9.34105253585761));
#13634=CARTESIAN_POINT('Ctrl Pts',(11.0038713507032,3.27808626456696,-9.48109547783808));
#13635=CARTESIAN_POINT('Ctrl Pts',(11.1958386868237,3.40738413972955,-9.62099443044572));
#13636=CARTESIAN_POINT('Ctrl Pts',(11.3869496174045,3.53610519063233,-9.76026926521936));
#13637=CARTESIAN_POINT('Ctrl Pts',(11.5790385083447,3.665337470246,-9.89940114828168));
#13638=CARTESIAN_POINT('Ctrl Pts',(11.7714345809803,3.79458803732612,-10.0380132338099));
#13639=CARTESIAN_POINT('Ctrl Pts',(11.9635224158196,3.92363153204024,-10.1764032488812));
#13640=CARTESIAN_POINT('Ctrl Pts',(12.155916448871,4.05269344373641,-10.314274892948));
#13641=CARTESIAN_POINT('Ctrl Pts',(12.3479491202722,4.18132152636456,-10.4512882521928));
#13642=CARTESIAN_POINT('Ctrl Pts',(12.53354535234,4.30563832776981,-10.5837092773927));
#13643=CARTESIAN_POINT('Ctrl Pts',(12.7188040406167,4.42955027592047,-10.7153286091806));
#13644=CARTESIAN_POINT('Ctrl Pts',(12.9031225251803,4.55268038845334,-10.8458735001829));
#13645=CARTESIAN_POINT('Ctrl Pts',(13.1554739610256,4.72125849263551,-11.0246032177404));
#13646=CARTESIAN_POINT('Ctrl Pts',(13.4103523866344,4.89121179563095,-11.2042784469551));
#13647=CARTESIAN_POINT('Ctrl Pts',(13.666596850669,5.06174747048535,-11.3841414734481));
#13648=CARTESIAN_POINT('Ctrl Pts',(13.9194672603251,5.23003764652439,-11.5616361848466));
#13649=CARTESIAN_POINT('Ctrl Pts',(14.1736679711021,5.39889509460814,-11.7393134647374));
#13650=CARTESIAN_POINT('Ctrl Pts',(14.4280832903348,5.56759036901465,-11.9164831860891));
#13651=CARTESIAN_POINT('Ctrl Pts',(14.6797373390532,5.7344547266017,-12.0917300140826));
#13652=CARTESIAN_POINT('Ctrl Pts',(14.9316013630457,5.90116059551977,-12.2664800265868));
#13653=CARTESIAN_POINT('Ctrl Pts',(15.182595603967,6.06703163029777,-12.4401067548795));
#13654=CARTESIAN_POINT('Ctrl Pts',(15.3891870324157,6.20355880274311,-12.5830175789813));
#13655=CARTESIAN_POINT('Ctrl Pts',(15.5951891994088,6.3395209766303,-12.725168121649));
#13656=CARTESIAN_POINT('Ctrl Pts',(15.8,6.47455487556025,-12.8662316724636));
#13657=CARTESIAN_POINT('Origin',(15.8,0.,0.));
#13658=CARTESIAN_POINT('',(15.8,10.1335518448686,-10.2357659846983));
#13659=CARTESIAN_POINT('Ctrl Pts',(10.0502525316942,5.21733945232202,-7.53128682236137));
#13660=CARTESIAN_POINT('Ctrl Pts',(10.2399700857355,5.38300672531024,-7.62691474601371));
#13661=CARTESIAN_POINT('Ctrl Pts',(10.432163929364,5.55055481152886,-7.72272706183542));
#13662=CARTESIAN_POINT('Ctrl Pts',(10.6261033397496,5.71924202232356,-7.81846533798032));
#13663=CARTESIAN_POINT('Ctrl Pts',(10.815494732926,5.88397339796269,-7.91195848340829));
#13664=CARTESIAN_POINT('Ctrl Pts',(11.0065507832434,6.04979105175912,-8.00538083967165));
#13665=CARTESIAN_POINT('Ctrl Pts',(11.1985909796548,6.21605213671196,-8.09850566734981));
#13666=CARTESIAN_POINT('Ctrl Pts',(11.3896566244822,6.38146949203575,-8.19115791194377));
#13667=CARTESIAN_POINT('Ctrl Pts',(11.5816964522024,6.54732580586942,-8.28351537255365));
#13668=CARTESIAN_POINT('Ctrl Pts',(11.7740402595052,6.71303622283071,-8.3753721282914));
#13669=CARTESIAN_POINT('Ctrl Pts',(11.9659830376824,6.87840114021723,-8.46703736637668));
#13670=CARTESIAN_POINT('Ctrl Pts',(12.1582285291931,7.04362087245244,-8.55820369955474));
#13671=CARTESIAN_POINT('Ctrl Pts',(12.3501107140342,7.20816146064372,-8.64868803888449));
#13672=CARTESIAN_POINT('Ctrl Pts',(12.5349837899974,7.36669167899046,-8.73586714908818));
#13673=CARTESIAN_POINT('Ctrl Pts',(12.7195196163977,7.52459184596093,-8.82241309395648));
#13674=CARTESIAN_POINT('Ctrl Pts',(12.9031225251803,7.68142427504574,-8.90818466253794));
#13675=CARTESIAN_POINT('Ctrl Pts',(13.046609999277,7.80399035667838,-8.97521598468133));
#13676=CARTESIAN_POINT('Ctrl Pts',(13.1909144693232,7.92707423833475,-9.04240096834747));
#13677=CARTESIAN_POINT('Ctrl Pts',(13.3358225135832,8.05049252087456,-9.10965124727546));
#13678=CARTESIAN_POINT('Ctrl Pts',(13.4722456635829,8.16668421304466,-9.17296377720826));
#13679=CARTESIAN_POINT('Ctrl Pts',(13.6092037742271,8.2831723388735,-9.23633418862365));
#13680=CARTESIAN_POINT('Ctrl Pts',(13.7465187613193,8.39980806233602,-9.29969102606761));
#13681=CARTESIAN_POINT('Ctrl Pts',(13.8831227642785,8.51583987394238,-9.36271981697347));
#13682=CARTESIAN_POINT('Ctrl Pts',(14.0200799576114,8.63201776215884,-9.42573515876483));
#13683=CARTESIAN_POINT('Ctrl Pts',(14.1572150090555,8.74819853760654,-9.48866882093701));
#13684=CARTESIAN_POINT('Ctrl Pts',(14.4088743845434,8.96140428686608,-9.6041596889));
#13685=CARTESIAN_POINT('Ctrl Pts',(14.661132727116,9.1746172658687,-9.71937357878233));
#13686=CARTESIAN_POINT('Ctrl Pts',(14.9129064697985,9.38698186590108,-9.83391026822726));
#13687=CARTESIAN_POINT('Ctrl Pts',(14.934810720465,9.40545753132288,-9.84387493066339));
#13688=CARTESIAN_POINT('Ctrl Pts',(14.9567113032167,9.42392680146146,-9.85383448723374));
#13689=CARTESIAN_POINT('Ctrl Pts',(14.9786075045277,9.44238912780876,-9.86378868594609));
#13690=CARTESIAN_POINT('Ctrl Pts',(15.1157365203996,9.55801286576868,-9.92612869889287));
#13691=CARTESIAN_POINT('Ctrl Pts',(15.252693690801,9.67336395156666,-9.98825831748495));
#13692=CARTESIAN_POINT('Ctrl Pts',(15.3893037522639,9.78830977806043,-10.0501174002428));
#13693=CARTESIAN_POINT('Ctrl Pts',(15.4578478923357,9.84598388161831,-10.0811552139138));
#13694=CARTESIAN_POINT('Ctrl Pts',(15.5263046465628,9.90355602888933,-10.1121249718658));
#13695=CARTESIAN_POINT('Ctrl Pts',(15.5946518761319,9.96100982960574,-10.1430193787867));
#13696=CARTESIAN_POINT('Ctrl Pts',(15.663218932117,10.0186484200082,-10.1740131519407));
#13697=CARTESIAN_POINT('Ctrl Pts',(15.7316757577788,10.076167877539,-10.2049310789385));
#13698=CARTESIAN_POINT('Ctrl Pts',(15.8,10.1335518448686,-10.2357659846983));
#13699=CARTESIAN_POINT('Origin',(15.8,0.,0.));
#13700=CARTESIAN_POINT('',(15.8,12.8006061549939,-6.60335220557564));
#13701=CARTESIAN_POINT('Ctrl Pts',(10.0502525316942,7.28928030147641,-5.55043285230422));
#13702=CARTESIAN_POINT('Ctrl Pts',(10.2399762236016,7.47639594802568,-5.59018769560145));
#13703=CARTESIAN_POINT('Ctrl Pts',(10.4321763653278,7.66535745978503,-5.62953666502917));
#13704=CARTESIAN_POINT('Ctrl Pts',(10.626122163118,7.85537951329466,-5.66846318065072));
#13705=CARTESIAN_POINT('Ctrl Pts',(10.8155134734694,8.04093922183132,-5.7064755732108));
#13706=CARTESIAN_POINT('Ctrl Pts',(11.006569415022,8.2275101466564,-5.74408496164232));
#13707=CARTESIAN_POINT('Ctrl Pts',(11.1986094788102,8.41441083753208,-5.78127435838112));
#13708=CARTESIAN_POINT('Ctrl Pts',(11.3896744033038,8.60036248577428,-5.81827491513835));
#13709=CARTESIAN_POINT('Ctrl Pts',(11.5817134810738,8.78664049259016,-5.85485947501094));
#13710=CARTESIAN_POINT('Ctrl Pts',(11.7740565170517,8.97262500016277,-5.89101292727606));
#13711=CARTESIAN_POINT('Ctrl Pts',(11.9659982062651,9.15822142880125,-5.9270909410361));
#13712=CARTESIAN_POINT('Ctrl Pts',(12.1582425865195,9.34352559234031,-5.96273934048964));
#13713=CARTESIAN_POINT('Ctrl Pts',(12.3501236493255,9.52797309682549,-5.99794900016104));
#13714=CARTESIAN_POINT('Ctrl Pts',(12.5349923977935,9.70567994717111,-6.03187191898507));
#13715=CARTESIAN_POINT('Ctrl Pts',(12.7195238985377,9.88259194572934,-6.06538737998544));
#13716=CARTESIAN_POINT('Ctrl Pts',(12.9031225251803,10.0582492231335,-6.09849633518511));
#13717=CARTESIAN_POINT('Ctrl Pts',(13.0466099992771,10.1955303101566,-6.12437191191713));
#13718=CARTESIAN_POINT('Ctrl Pts',(13.1909144693232,10.3333513349338,-6.15023362158894));
#13719=CARTESIAN_POINT('Ctrl Pts',(13.3358225135832,10.4715105676525,-6.17605409599263));
#13720=CARTESIAN_POINT('Ctrl Pts',(13.4722456635829,10.6015800736297,-6.20036268749027));
#13721=CARTESIAN_POINT('Ctrl Pts',(13.6092037742271,10.7319493881454,-6.22463472522239));
#13722=CARTESIAN_POINT('Ctrl Pts',(13.7465187613193,10.8624548834565,-6.24884824365307));
#13723=CARTESIAN_POINT('Ctrl Pts',(13.8831227642785,10.9922846525529,-6.27293639028148));
#13724=CARTESIAN_POINT('Ctrl Pts',(14.0200799576114,11.1222491940658,-6.29696660630782));
#13725=CARTESIAN_POINT('Ctrl Pts',(14.1572150090555,11.2521912379382,-6.32091824773854));
#13726=CARTESIAN_POINT('Ctrl Pts',(14.408895707,11.4906707801833,-6.36487612552926));
#13727=CARTESIAN_POINT('Ctrl Pts',(14.6611754735313,11.7290715847961,-6.40856830116405));
#13728=CARTESIAN_POINT('Ctrl Pts',(14.9129704662278,11.9664560266743,-6.45187850892383));
#13729=CARTESIAN_POINT('Ctrl Pts',(14.9348533776098,11.9870865509331,-6.45564249735026));
#13730=CARTESIAN_POINT('Ctrl Pts',(14.9567326275241,12.0077094295123,-6.45940361158516));
#13731=CARTESIAN_POINT('Ctrl Pts',(14.9786075045277,12.0283240646364,-6.46316178167156));
#13732=CARTESIAN_POINT('Ctrl Pts',(15.1157365203996,12.1575528884896,-6.48672096169998));
#13733=CARTESIAN_POINT('Ctrl Pts',(15.252693690801,12.2864573923713,-6.5101642983752));
#13734=CARTESIAN_POINT('Ctrl Pts',(15.3893037522639,12.4148928744451,-6.53347557107031));
#13735=CARTESIAN_POINT('Ctrl Pts',(15.4578478923357,12.4793354168112,-6.54517200926641));
#13736=CARTESIAN_POINT('Ctrl Pts',(15.5263046465628,12.5436599631772,-6.5568352285584));
#13737=CARTESIAN_POINT('Ctrl Pts',(15.5946518761319,12.6078486707221,-6.56846335549623));
#13738=CARTESIAN_POINT('Ctrl Pts',(15.663218932117,12.6722438295541,-6.58012888218654));
#13739=CARTESIAN_POINT('Ctrl Pts',(15.7316757577788,12.7365022490344,-6.59175908863286));
#13740=CARTESIAN_POINT('Ctrl Pts',(15.8,12.8006061549939,-6.60335220557564));
#13741=CARTESIAN_POINT('Origin',(15.8,0.,0.));
#13742=CARTESIAN_POINT('',(15.8,14.2372609598209,2.18178336415567));
#13743=CARTESIAN_POINT('Ctrl Pts',(10.0502525316942,9.15961421508102,-0.20586304261726));
#13744=CARTESIAN_POINT('Ctrl Pts',(10.2391570234258,9.33360673051055,-0.128377591099454));
#13745=CARTESIAN_POINT('Ctrl Pts',(10.430516625224,9.50884304477959,-0.0494911083978059));
#13746=CARTESIAN_POINT('Ctrl Pts',(10.6236099689116,9.68468614630322,0.0303537569977821));
#13747=CARTESIAN_POINT('Ctrl Pts',(10.8129280637645,9.85709126570154,0.108637541989021));
#13748=CARTESIAN_POINT('Ctrl Pts',(11.0039127690159,10.0300795089048,0.187842691358935));
#13749=CARTESIAN_POINT('Ctrl Pts',(11.1958842059477,10.2030901320274,0.267582809353735));
#13750=CARTESIAN_POINT('Ctrl Pts',(11.3869971487108,10.3753270535335,0.346966330412031));
#13751=CARTESIAN_POINT('Ctrl Pts',(11.579088017581,10.5475859558081,0.426880221764355));
#13752=CARTESIAN_POINT('Ctrl Pts',(11.7714860143417,10.7193560970322,0.506972115618906));
#13753=CARTESIAN_POINT('Ctrl Pts',(11.9635738218519,10.8908493057922,0.586934883157515));
#13754=CARTESIAN_POINT('Ctrl Pts',(12.1559677677312,11.0618551603493,0.667075331863697));
#13755=CARTESIAN_POINT('Ctrl Pts',(12.3480002929717,11.2319106356085,0.747068390651361));
#13756=CARTESIAN_POINT('Ctrl Pts',(12.5335794054256,11.3962512551312,0.824373216142209));
#13757=CARTESIAN_POINT('Ctrl Pts',(12.7188209807523,11.5597044367662,0.901540748122834));
#13758=CARTESIAN_POINT('Ctrl Pts',(12.9031225251803,11.7218943942307,0.978296811887802));
#13759=CARTESIAN_POINT('Ctrl Pts',(13.1554719876668,11.9439682173986,1.08339279192306));
#13760=CARTESIAN_POINT('Ctrl Pts',(13.4103484003956,12.1673662092149,1.18950448019821));
#13761=CARTESIAN_POINT('Ctrl Pts',(13.666590839264,12.3911227672744,1.29611200619563));
#13762=CARTESIAN_POINT('Ctrl Pts',(13.9194596713251,12.6119334173462,1.40131597126461));
#13763=CARTESIAN_POINT('Ctrl Pts',(14.1736587969712,12.8330929959789,1.50700303047468));
#13764=CARTESIAN_POINT('Ctrl Pts',(14.4280725441392,13.053719762021,1.61269270111584));
#13765=CARTESIAN_POINT('Ctrl Pts',(14.6797279548917,13.271954507782,1.71723649158925));
#13766=CARTESIAN_POINT('Ctrl Pts',(14.9315933585706,13.4896677845255,1.82178307810091));
#13767=CARTESIAN_POINT('Ctrl Pts',(15.1825889792217,13.7060547738705,1.9258827920696));
#13768=CARTESIAN_POINT('Ctrl Pts',(15.3891826285161,13.8841621753965,2.01156691573479));
#13769=CARTESIAN_POINT('Ctrl Pts',(15.5951870101935,14.0613719009692,2.09694862236039));
#13770=CARTESIAN_POINT('Ctrl Pts',(15.8,14.2372609598209,2.18178336415567));
#13771=CARTESIAN_POINT('Origin',(15.8,0.,0.));
#13772=CARTESIAN_POINT('',(15.8,12.8662316724636,6.47455487556026));
#13773=CARTESIAN_POINT('Ctrl Pts',(10.0502525316942,8.77492596468499,2.63468906623289));
#13774=CARTESIAN_POINT('Ctrl Pts',(10.2391461906124,8.91645024269597,2.76214144474541));
#13775=CARTESIAN_POINT('Ctrl Pts',(10.4304946780266,9.05872439496881,2.89131047500261));
#13776=CARTESIAN_POINT('Ctrl Pts',(10.6235767498538,9.20127947078389,3.02157840065296));
#13777=CARTESIAN_POINT('Ctrl Pts',(10.8128907594439,9.34105253585702,3.14930410347176));
#13778=CARTESIAN_POINT('Ctrl Pts',(11.0038713507024,9.48109547783751,3.27808626456643));
#13779=CARTESIAN_POINT('Ctrl Pts',(11.195838686823,9.62099443044516,3.40738413972904));
#13780=CARTESIAN_POINT('Ctrl Pts',(11.3869496174036,9.76026926521869,3.53610519063172));
#13781=CARTESIAN_POINT('Ctrl Pts',(11.5790385083437,9.89940114828092,3.6653374702453));
#13782=CARTESIAN_POINT('Ctrl Pts',(11.7714345809791,10.0380132338091,3.79458803732532));
#13783=CARTESIAN_POINT('Ctrl Pts',(11.9635224158183,10.1764032488802,3.92363153203936));
#13784=CARTESIAN_POINT('Ctrl Pts',(12.1559164488696,10.314274892947,4.05269344373545));
#13785=CARTESIAN_POINT('Ctrl Pts',(12.3479491202706,10.4512882521917,4.18132152636351));
#13786=CARTESIAN_POINT('Ctrl Pts',(12.533545352339,10.5837092773919,4.30563832776911));
#13787=CARTESIAN_POINT('Ctrl Pts',(12.7188040406162,10.7153286091803,4.42955027592013));
#13788=CARTESIAN_POINT('Ctrl Pts',(12.9031225251803,10.8458735001829,4.55268038845334));
#13789=CARTESIAN_POINT('Ctrl Pts',(13.155473961026,11.0246032177407,4.72125849263582));
#13790=CARTESIAN_POINT('Ctrl Pts',(13.4103523866354,11.2042784469558,4.89121179563158));
#13791=CARTESIAN_POINT('Ctrl Pts',(13.6665968506704,11.3841414734491,5.0617474704863));
#13792=CARTESIAN_POINT('Ctrl Pts',(13.9194672603269,11.5616361848478,5.2300376465256));
#13793=CARTESIAN_POINT('Ctrl Pts',(14.1736679711043,11.7393134647389,5.3988950946096));
#13794=CARTESIAN_POINT('Ctrl Pts',(14.4280832903373,11.9164831860909,5.56759036901635));
#13795=CARTESIAN_POINT('Ctrl Pts',(14.6797373390571,12.0917300140853,5.73445472660428));
#13796=CARTESIAN_POINT('Ctrl Pts',(14.9316013630509,12.2664800265904,5.90116059552322));
#13797=CARTESIAN_POINT('Ctrl Pts',(15.1825956039735,12.440106754884,6.06703163030206));
#13798=CARTESIAN_POINT('Ctrl Pts',(15.3891870324201,12.5830175789843,6.20355880274597));
#13799=CARTESIAN_POINT('Ctrl Pts',(15.5951891994109,12.7251681216505,6.33952097663173));
#13800=CARTESIAN_POINT('Ctrl Pts',(15.8,12.8662316724636,6.47455487556026));
#13801=CARTESIAN_POINT('Origin',(15.8,0.,0.));
#13802=CARTESIAN_POINT('',(15.8,10.2357659846983,10.1335518448686));
#13803=CARTESIAN_POINT('Ctrl Pts',(10.0502525316942,7.53128682236137,5.21733945232202));
#13804=CARTESIAN_POINT('Ctrl Pts',(10.2399700857352,7.62691474601355,5.38300672530997));
#13805=CARTESIAN_POINT('Ctrl Pts',(10.4321639293634,7.72272706183511,5.55055481152831));
#13806=CARTESIAN_POINT('Ctrl Pts',(10.6261033397486,7.81846533797985,5.71924202232274));
#13807=CARTESIAN_POINT('Ctrl Pts',(10.8154947329249,7.91195848340778,5.8839733979618));
#13808=CARTESIAN_POINT('Ctrl Pts',(11.0065507832423,8.00538083967111,6.04979105175817));
#13809=CARTESIAN_POINT('Ctrl Pts',(11.1985909796536,8.09850566734924,6.21605213671094));
#13810=CARTESIAN_POINT('Ctrl Pts',(11.3896566244812,8.19115791194327,6.38146949203487));
#13811=CARTESIAN_POINT('Ctrl Pts',(11.5816964522015,8.28351537255324,6.54732580586867));
#13812=CARTESIAN_POINT('Ctrl Pts',(11.7740402595045,8.37537212829106,6.71303622283009));
#13813=CARTESIAN_POINT('Ctrl Pts',(11.9659830376819,8.46703736637644,6.87840114021681));
#13814=CARTESIAN_POINT('Ctrl Pts',(12.1582285291928,8.55820369955461,7.04362087245221));
#13815=CARTESIAN_POINT('Ctrl Pts',(12.3501107140342,8.64868803888447,7.20816146064368));
#13816=CARTESIAN_POINT('Ctrl Pts',(12.5349837899973,8.73586714908816,7.36669167899044));
#13817=CARTESIAN_POINT('Ctrl Pts',(12.7195196163976,8.82241309395647,7.52459184596092));
#13818=CARTESIAN_POINT('Ctrl Pts',(12.9031225251803,8.90818466253794,7.68142427504575));
#13819=CARTESIAN_POINT('Ctrl Pts',(13.0466099992771,8.97521598468133,7.80399035667839));
#13820=CARTESIAN_POINT('Ctrl Pts',(13.1909144693232,9.04240096834747,7.92707423833476));
#13821=CARTESIAN_POINT('Ctrl Pts',(13.3358225135832,9.10965124727546,8.05049252087456));
#13822=CARTESIAN_POINT('Ctrl Pts',(13.4722456635829,9.17296377720826,8.16668421304467));
#13823=CARTESIAN_POINT('Ctrl Pts',(13.6092037742271,9.23633418862365,8.2831723388735));
#13824=CARTESIAN_POINT('Ctrl Pts',(13.7465187613193,9.29969102606761,8.39980806233602));
#13825=CARTESIAN_POINT('Ctrl Pts',(13.8831227642785,9.36271981697347,8.51583987394238));
#13826=CARTESIAN_POINT('Ctrl Pts',(14.0200799576114,9.42573515876482,8.63201776215885));
#13827=CARTESIAN_POINT('Ctrl Pts',(14.1572150090555,9.48866882093701,8.74819853760654));
#13828=CARTESIAN_POINT('Ctrl Pts',(14.408874384546,9.6041596889012,8.9614042868683));
#13829=CARTESIAN_POINT('Ctrl Pts',(14.6611327271213,9.71937357878472,9.17461726587313));
#13830=CARTESIAN_POINT('Ctrl Pts',(14.9129064698064,9.83391026823084,9.38698186590772));
#13831=CARTESIAN_POINT('Ctrl Pts',(14.9348107204702,9.84387493066577,9.40545753132731));
#13832=CARTESIAN_POINT('Ctrl Pts',(14.9567113032193,9.85383448723492,9.42392680146367));
#13833=CARTESIAN_POINT('Ctrl Pts',(14.9786075045277,9.86378868594609,9.44238912780876));
#13834=CARTESIAN_POINT('Ctrl Pts',(15.1157365203996,9.92612869889287,9.55801286576868));
#13835=CARTESIAN_POINT('Ctrl Pts',(15.252693690801,9.98825831748494,9.67336395156666));
#13836=CARTESIAN_POINT('Ctrl Pts',(15.3893037522639,10.0501174002428,9.78830977806044));
#13837=CARTESIAN_POINT('Ctrl Pts',(15.4578478923357,10.0811552139138,9.84598388161831));
#13838=CARTESIAN_POINT('Ctrl Pts',(15.5263046465628,10.1121249718658,9.90355602888934));
#13839=CARTESIAN_POINT('Ctrl Pts',(15.5946518761319,10.1430193787867,9.96100982960575));
#13840=CARTESIAN_POINT('Ctrl Pts',(15.663218932117,10.1740131519407,10.0186484200082));
#13841=CARTESIAN_POINT('Ctrl Pts',(15.7316757577788,10.2049310789384,10.076167877539));
#13842=CARTESIAN_POINT('Ctrl Pts',(15.8,10.2357659846983,10.1335518448686));
#13843=CARTESIAN_POINT('Origin',(15.8,0.,0.));
#13844=CARTESIAN_POINT('',(15.8,6.60335220557564,12.8006061549939));
#13845=CARTESIAN_POINT('Ctrl Pts',(10.0502525316942,5.55043285230422,7.28928030147641));
#13846=CARTESIAN_POINT('Ctrl Pts',(10.2399762236018,5.59018769560149,7.47639594802589));
#13847=CARTESIAN_POINT('Ctrl Pts',(10.4321763653283,5.62953666502926,7.66535745978546));
#13848=CARTESIAN_POINT('Ctrl Pts',(10.6261221631187,5.66846318065085,7.85537951329531));
#13849=CARTESIAN_POINT('Ctrl Pts',(10.8155134734701,5.70647557321093,8.040939221832));
#13850=CARTESIAN_POINT('Ctrl Pts',(11.0065694150227,5.74408496164246,8.22751014665713));
#13851=CARTESIAN_POINT('Ctrl Pts',(11.198609478811,5.78127435838126,8.41441083753284));
#13852=CARTESIAN_POINT('Ctrl Pts',(11.3896744033045,5.81827491513847,8.60036248577492));
#13853=CARTESIAN_POINT('Ctrl Pts',(11.5817134810743,5.85485947501103,8.78664049259069));
#13854=CARTESIAN_POINT('Ctrl Pts',(11.7740565170522,5.89101292727613,8.97262500016317));
#13855=CARTESIAN_POINT('Ctrl Pts',(11.9659982062654,5.92709094103616,9.15822142880157));
#13856=CARTESIAN_POINT('Ctrl Pts',(12.1582425865198,5.96273934048968,9.34352559234053));
#13857=CARTESIAN_POINT('Ctrl Pts',(12.3501236493256,5.99794900016105,9.5279730968256));
#13858=CARTESIAN_POINT('Ctrl Pts',(12.5349923977936,6.03187191898508,9.7056799471712));
#13859=CARTESIAN_POINT('Ctrl Pts',(12.7195238985378,6.06538737998545,9.8825919457294));
#13860=CARTESIAN_POINT('Ctrl Pts',(12.9031225251803,6.0984963351851,10.0582492231335));
#13861=CARTESIAN_POINT('Ctrl Pts',(13.0466099992771,6.12437191191712,10.1955303101566));
#13862=CARTESIAN_POINT('Ctrl Pts',(13.1909144693232,6.15023362158894,10.3333513349338));
#13863=CARTESIAN_POINT('Ctrl Pts',(13.3358225135832,6.17605409599263,10.4715105676525));
#13864=CARTESIAN_POINT('Ctrl Pts',(13.4722456635829,6.20036268749026,10.6015800736297));
#13865=CARTESIAN_POINT('Ctrl Pts',(13.6092037742271,6.22463472522239,10.7319493881454));
#13866=CARTESIAN_POINT('Ctrl Pts',(13.7465187613193,6.24884824365306,10.8624548834565));
#13867=CARTESIAN_POINT('Ctrl Pts',(13.8831227642785,6.27293639028147,10.9922846525529));
#13868=CARTESIAN_POINT('Ctrl Pts',(14.0200799576114,6.29696660630781,11.1222491940658));
#13869=CARTESIAN_POINT('Ctrl Pts',(14.1572150090555,6.32091824773854,11.2521912379382));
#13870=CARTESIAN_POINT('Ctrl Pts',(14.4088957069953,6.36487612552845,11.4906707801789));
#13871=CARTESIAN_POINT('Ctrl Pts',(14.6611754735221,6.40856830116244,11.7290715847874));
#13872=CARTESIAN_POINT('Ctrl Pts',(14.912970466214,6.45187850892146,11.9664560266613));
#13873=CARTESIAN_POINT('Ctrl Pts',(14.9348533776006,6.45564249734868,11.9870865509245));
#13874=CARTESIAN_POINT('Ctrl Pts',(14.9567326275195,6.45940361158437,12.007709429508));
#13875=CARTESIAN_POINT('Ctrl Pts',(14.9786075045277,6.46316178167156,12.0283240646364));
#13876=CARTESIAN_POINT('Ctrl Pts',(15.1157365203996,6.48672096169998,12.1575528884896));
#13877=CARTESIAN_POINT('Ctrl Pts',(15.252693690801,6.5101642983752,12.2864573923713));
#13878=CARTESIAN_POINT('Ctrl Pts',(15.3893037522639,6.53347557107031,12.4148928744451));
#13879=CARTESIAN_POINT('Ctrl Pts',(15.4578478923357,6.54517200926641,12.4793354168112));
#13880=CARTESIAN_POINT('Ctrl Pts',(15.5263046465628,6.5568352285584,12.5436599631772));
#13881=CARTESIAN_POINT('Ctrl Pts',(15.5946518761319,6.56846335549623,12.6078486707221));
#13882=CARTESIAN_POINT('Ctrl Pts',(15.663218932117,6.58012888218654,12.6722438295541));
#13883=CARTESIAN_POINT('Ctrl Pts',(15.7316757577788,6.59175908863285,12.7365022490344));
#13884=CARTESIAN_POINT('Ctrl Pts',(15.8,6.60335220557564,12.8006061549939));
#13885=CARTESIAN_POINT('Origin',(15.8,0.,0.));
#13886=CARTESIAN_POINT('',(15.8,2.32455630431103,14.2146479476009));
#13887=CARTESIAN_POINT('Ctrl Pts',(10.0502525316942,3.02626384252387,8.64769560732005));
#13888=CARTESIAN_POINT('Ctrl Pts',(10.239953859285,3.00625338967616,8.83791565898891));
#13889=CARTESIAN_POINT('Ctrl Pts',(10.4321310528894,2.98528677263253,9.02976542249209));
#13890=CARTESIAN_POINT('Ctrl Pts',(10.6260535771563,2.96359080496254,9.22249314017983));
#13891=CARTESIAN_POINT('Ctrl Pts',(10.8154434277094,2.94240195085619,9.41071611112315));
#13892=CARTESIAN_POINT('Ctrl Pts',(11.0064979730127,2.9205173235086,9.5997763303737));
#13893=CARTESIAN_POINT('Ctrl Pts',(11.1985367155039,2.89813133617991,9.78902046263069));
#13894=CARTESIAN_POINT('Ctrl Pts',(11.3896029988914,2.87585870856653,9.97730628732497));
#13895=CARTESIAN_POINT('Ctrl Pts',(11.5816435370124,2.85308955972943,10.1657740234633));
#13896=CARTESIAN_POINT('Ctrl Pts',(11.7739881178962,2.83000106681665,10.353829469752));
#13897=CARTESIAN_POINT('Ctrl Pts',(11.9659332365641,2.80696052420482,10.5414943615216));
#13898=CARTESIAN_POINT('Ctrl Pts',(12.1581811364309,2.78360167031431,10.7287485903504));
#13899=CARTESIAN_POINT('Ctrl Pts',(12.3500657725588,2.76009024231686,10.9150525380981));
#13900=CARTESIAN_POINT('Ctrl Pts',(12.5349538836675,2.73743609136639,11.0945634446837));
#13901=CARTESIAN_POINT('Ctrl Pts',(12.7195047388313,2.71463999548723,11.2731923646037));
#13902=CARTESIAN_POINT('Ctrl Pts',(12.9031225251803,2.69184501333336,11.4505020946774));
#13903=CARTESIAN_POINT('Ctrl Pts',(13.0466099992771,2.67403195460754,11.5890601603578));
#13904=CARTESIAN_POINT('Ctrl Pts',(13.1909144693232,2.65603885317597,11.7281274609627));
#13905=CARTESIAN_POINT('Ctrl Pts',(13.3358225135832,2.63790201856914,11.8675036836248));
#13906=CARTESIAN_POINT('Ctrl Pts',(13.4722456635829,2.62082716174719,11.9987189203477));
#13907=CARTESIAN_POINT('Ctrl Pts',(13.6092037742272,2.60362489076148,12.1302080042448));
#13908=CARTESIAN_POINT('Ctrl Pts',(13.7465187613194,2.58632488288814,12.2618085151784));
#13909=CARTESIAN_POINT('Ctrl Pts',(13.8831227642785,2.56911445031434,12.3927276301685));
#13910=CARTESIAN_POINT('Ctrl Pts',(14.0200799576114,2.55180727580019,12.5237570157981));
#13911=CARTESIAN_POINT('Ctrl Pts',(14.1572150090555,2.53443232271127,12.6547407331994));
#13912=CARTESIAN_POINT('Ctrl Pts',(14.4088349682213,2.50255218017508,12.8950740198159));
#13913=CARTESIAN_POINT('Ctrl Pts',(14.6610537068593,2.47044377568191,13.1352504185273));
#13914=CARTESIAN_POINT('Ctrl Pts',(14.912788167058,2.4382861620121,13.374342879882));
#13915=CARTESIAN_POINT('Ctrl Pts',(14.9347318651876,2.43548298215988,13.3951845747094));
#13916=CARTESIAN_POINT('Ctrl Pts',(14.956671883473,2.43267942911465,13.4160180659855));
#13917=CARTESIAN_POINT('Ctrl Pts',(14.9786075045277,2.42987562206087,13.4368427586266));
#13918=CARTESIAN_POINT('Ctrl Pts',(15.1157365203996,2.4123478164419,13.5670268824575));
#13919=CARTESIAN_POINT('Ctrl Pts',(15.252693690801,2.39481006097156,13.6968667539964));
#13920=CARTESIAN_POINT('Ctrl Pts',(15.3893037522639,2.3772916450855,13.8262197421006));
#13921=CARTESIAN_POINT('Ctrl Pts',(15.4578478923357,2.368501774563,13.8911226433977));
#13922=CARTESIAN_POINT('Ctrl Pts',(15.5263046465628,2.35971677469615,13.9559030572658));
#13923=CARTESIAN_POINT('Ctrl Pts',(15.5946518761319,2.3509403772656,14.0205434363407));
#13924=CARTESIAN_POINT('Ctrl Pts',(15.663218932117,2.34213575215115,14.085391719422));
#13925=CARTESIAN_POINT('Ctrl Pts',(15.7316757577788,2.33333979124571,14.1500990399651));
#13926=CARTESIAN_POINT('Ctrl Pts',(15.8,2.32455630431103,14.2146479476009));
#13927=CARTESIAN_POINT('Origin',(15.8,0.,0.));
#13928=CARTESIAN_POINT('',(15.8,-2.18178336415567,14.2372609598209));
#13929=CARTESIAN_POINT('Ctrl Pts',(10.0502525316942,0.205863042617261,9.15961421508102));
#13930=CARTESIAN_POINT('Ctrl Pts',(10.2391570234259,0.128377591099419,9.33360673051063));
#13931=CARTESIAN_POINT('Ctrl Pts',(10.4305166252242,0.0494911083977331,
9.50884304477974));
#13932=CARTESIAN_POINT('Ctrl Pts',(10.6236099689119,-0.0303537569978928,
9.68468614630346));
#13933=CARTESIAN_POINT('Ctrl Pts',(10.8129280637648,-0.108637541989135,
9.85709126570178));
#13934=CARTESIAN_POINT('Ctrl Pts',(11.0039127690162,-0.187842691359053,
10.0300795089051));
#13935=CARTESIAN_POINT('Ctrl Pts',(11.195884205948,-0.267582809353856,10.2030901320277));
#13936=CARTESIAN_POINT('Ctrl Pts',(11.3869971487111,-0.34696633041216,10.3753270535338));
#13937=CARTESIAN_POINT('Ctrl Pts',(11.5790880175814,-0.426880221764492,
10.5475859558084));
#13938=CARTESIAN_POINT('Ctrl Pts',(11.771486014342,-0.50697211561905,10.7193560970325));
#13939=CARTESIAN_POINT('Ctrl Pts',(11.9635738218523,-0.586934883157645,
10.8908493057925));
#13940=CARTESIAN_POINT('Ctrl Pts',(12.1559677677314,-0.667075331863813,
11.0618551603495));
#13941=CARTESIAN_POINT('Ctrl Pts',(12.348000292972,-0.747068390651463,11.2319106356087));
#13942=CARTESIAN_POINT('Ctrl Pts',(12.5335794054258,-0.824373216142277,
11.3962512551313));
#13943=CARTESIAN_POINT('Ctrl Pts',(12.7188209807524,-0.901540748122868,
11.5597044367663));
#13944=CARTESIAN_POINT('Ctrl Pts',(12.9031225251803,-0.978296811887801,
11.7218943942307));
#13945=CARTESIAN_POINT('Ctrl Pts',(13.1554719876673,-1.08339279192325,11.943968217399));
#13946=CARTESIAN_POINT('Ctrl Pts',(13.4103484003965,-1.18950448019859,12.1673662092157));
#13947=CARTESIAN_POINT('Ctrl Pts',(13.6665908392654,-1.29611200619622,12.3911227672756));
#13948=CARTESIAN_POINT('Ctrl Pts',(13.9194596713268,-1.40131597126529,12.6119334173477));
#13949=CARTESIAN_POINT('Ctrl Pts',(14.1736587969731,-1.50700303047547,12.8330929959806));
#13950=CARTESIAN_POINT('Ctrl Pts',(14.4280725441414,-1.61269270111672,13.0537197620228));
#13951=CARTESIAN_POINT('Ctrl Pts',(14.6797279548927,-1.71723649158967,13.2719545077828));
#13952=CARTESIAN_POINT('Ctrl Pts',(14.9315933585705,-1.82178307810086,13.4896677845254));
#13953=CARTESIAN_POINT('Ctrl Pts',(15.1825889792205,-1.92588279206909,13.7060547738694));
#13954=CARTESIAN_POINT('Ctrl Pts',(15.3891826285153,-2.01156691573445,13.8841621753958));
#13955=CARTESIAN_POINT('Ctrl Pts',(15.5951870101931,-2.09694862236022,14.0613719009688));
#13956=CARTESIAN_POINT('Ctrl Pts',(15.8,-2.18178336415567,14.2372609598209));
#13957=CARTESIAN_POINT('Origin',(15.8,0.,0.));
#13958=CARTESIAN_POINT('',(15.8,-6.47455487556026,12.8662316724636));
#13959=CARTESIAN_POINT('Ctrl Pts',(10.0502525316942,-2.63468906623289,8.77492596468499));
#13960=CARTESIAN_POINT('Ctrl Pts',(10.2391461906128,-2.76214144474569,8.91645024269629));
#13961=CARTESIAN_POINT('Ctrl Pts',(10.4304946780274,-2.89131047500319,9.05872439496945));
#13962=CARTESIAN_POINT('Ctrl Pts',(10.6235767498551,-3.02157840065384,9.20127947078485));
#13963=CARTESIAN_POINT('Ctrl Pts',(10.8128907594452,-3.1493041034726,9.34105253585794));
#13964=CARTESIAN_POINT('Ctrl Pts',(11.0038713507036,-3.27808626456724,9.48109547783839));
#13965=CARTESIAN_POINT('Ctrl Pts',(11.1958386868241,-3.40738413972981,9.620994430446));
#13966=CARTESIAN_POINT('Ctrl Pts',(11.3869496174047,-3.53610519063243,9.76026926521946));
#13967=CARTESIAN_POINT('Ctrl Pts',(11.5790385083446,-3.66533747024595,9.89940114828162));
#13968=CARTESIAN_POINT('Ctrl Pts',(11.77143458098,-3.79458803732591,10.0380132338097));
#13969=CARTESIAN_POINT('Ctrl Pts',(11.9635224158189,-3.92363153203981,10.1764032488807));
#13970=CARTESIAN_POINT('Ctrl Pts',(12.15591644887,-4.05269344373575,10.3142748929473));
#13971=CARTESIAN_POINT('Ctrl Pts',(12.3479491202708,-4.18132152636367,10.4512882521919));
#13972=CARTESIAN_POINT('Ctrl Pts',(12.5335453523391,-4.30563832776922,10.583709277392));
#13973=CARTESIAN_POINT('Ctrl Pts',(12.7188040406163,-4.42955027592018,10.7153286091803));
#13974=CARTESIAN_POINT('Ctrl Pts',(12.9031225251803,-4.55268038845334,10.8458735001828));
#13975=CARTESIAN_POINT('Ctrl Pts',(13.1554739610255,-4.72125849263545,11.0246032177403));
#13976=CARTESIAN_POINT('Ctrl Pts',(13.4103523866342,-4.89121179563083,11.204278446955));
#13977=CARTESIAN_POINT('Ctrl Pts',(13.6665968506687,-5.06174747048518,11.3841414734479));
#13978=CARTESIAN_POINT('Ctrl Pts',(13.919467260325,-5.23003764652437,11.5616361848466));
#13979=CARTESIAN_POINT('Ctrl Pts',(14.1736679711023,-5.39889509460827,11.7393134647375));
#13980=CARTESIAN_POINT('Ctrl Pts',(14.4280832903352,-5.56759036901493,11.9164831860894));
#13981=CARTESIAN_POINT('Ctrl Pts',(14.6797373390547,-5.7344547266027,12.0917300140837));
#13982=CARTESIAN_POINT('Ctrl Pts',(14.9316013630483,-5.90116059552149,12.2664800265886));
#13983=CARTESIAN_POINT('Ctrl Pts',(15.1825956039707,-6.06703163030022,12.4401067548821));
#13984=CARTESIAN_POINT('Ctrl Pts',(15.3891870324182,-6.20355880274473,12.583017578983));
#13985=CARTESIAN_POINT('Ctrl Pts',(15.59518919941,-6.3395209766311,12.7251681216498));
#13986=CARTESIAN_POINT('Ctrl Pts',(15.8,-6.47455487556026,12.8662316724636));
#13987=CARTESIAN_POINT('Origin',(15.8,0.,0.));
#13988=CARTESIAN_POINT('',(15.8,-10.1335518448686,10.2357659846983));
#13989=CARTESIAN_POINT('Ctrl Pts',(10.0502525316942,-5.21733945232202,7.53128682236137));
#13990=CARTESIAN_POINT('Ctrl Pts',(10.2399700857352,-5.38300672530999,7.62691474601356));
#13991=CARTESIAN_POINT('Ctrl Pts',(10.4321639293634,-5.55055481152835,7.72272706183513));
#13992=CARTESIAN_POINT('Ctrl Pts',(10.6261033397487,-5.71924202232279,7.81846533797988));
#13993=CARTESIAN_POINT('Ctrl Pts',(10.815494732925,-5.88397339796186,7.91195848340782));
#13994=CARTESIAN_POINT('Ctrl Pts',(11.0065507832424,-6.04979105175824,8.00538083967115));
#13995=CARTESIAN_POINT('Ctrl Pts',(11.1985909796537,-6.21605213671102,8.09850566734929));
#13996=CARTESIAN_POINT('Ctrl Pts',(11.3896566244815,-6.38146949203515,8.19115791194343));
#13997=CARTESIAN_POINT('Ctrl Pts',(11.5816964522021,-6.54732580586915,8.2835153725535));
#13998=CARTESIAN_POINT('Ctrl Pts',(11.7740402595053,-6.71303622283077,8.37537212829144));
#13999=CARTESIAN_POINT('Ctrl Pts',(11.9659830376826,-6.87840114021745,8.4670373663768));
#14000=CARTESIAN_POINT('Ctrl Pts',(12.1582285291935,-7.0436208724528,8.55820369955494));
#14001=CARTESIAN_POINT('Ctrl Pts',(12.3501107140348,-7.20816146064422,8.64868803888477));
#14002=CARTESIAN_POINT('Ctrl Pts',(12.5349837899977,-7.3666916789908,8.73586714908836));
#14003=CARTESIAN_POINT('Ctrl Pts',(12.7195196163979,-7.5245918459611,8.82241309395657));
#14004=CARTESIAN_POINT('Ctrl Pts',(12.9031225251803,-7.68142427504574,8.90818466253794));
#14005=CARTESIAN_POINT('Ctrl Pts',(13.0466099992771,-7.80399035667839,8.97521598468134));
#14006=CARTESIAN_POINT('Ctrl Pts',(13.1909144693232,-7.92707423833475,9.04240096834747));
#14007=CARTESIAN_POINT('Ctrl Pts',(13.3358225135832,-8.05049252087456,9.10965124727546));
#14008=CARTESIAN_POINT('Ctrl Pts',(13.4722456635829,-8.16668421304467,9.17296377720826));
#14009=CARTESIAN_POINT('Ctrl Pts',(13.6092037742271,-8.2831723388735,9.23633418862365));
#14010=CARTESIAN_POINT('Ctrl Pts',(13.7465187613193,-8.39980806233602,9.29969102606761));
#14011=CARTESIAN_POINT('Ctrl Pts',(13.8831227642785,-8.51583987394238,9.36271981697347));
#14012=CARTESIAN_POINT('Ctrl Pts',(14.0200799576114,-8.63201776215885,9.42573515876482));
#14013=CARTESIAN_POINT('Ctrl Pts',(14.1572150090555,-8.74819853760654,9.48866882093701));
#14014=CARTESIAN_POINT('Ctrl Pts',(14.4088743845451,-8.96140428686748,9.60415968890076));
#14015=CARTESIAN_POINT('Ctrl Pts',(14.6611327271194,-9.17461726587151,9.71937357878384));
#14016=CARTESIAN_POINT('Ctrl Pts',(14.9129064698035,-9.38698186590529,9.83391026822953));
#14017=CARTESIAN_POINT('Ctrl Pts',(14.9348107204683,-9.40545753132569,9.8438749306649));
#14018=CARTESIAN_POINT('Ctrl Pts',(14.9567113032183,-9.42392680146286,9.85383448723449));
#14019=CARTESIAN_POINT('Ctrl Pts',(14.9786075045277,-9.44238912780876,9.86378868594609));
#14020=CARTESIAN_POINT('Ctrl Pts',(15.1157365203996,-9.55801286576868,9.92612869889287));
#14021=CARTESIAN_POINT('Ctrl Pts',(15.252693690801,-9.67336395156666,9.98825831748495));
#14022=CARTESIAN_POINT('Ctrl Pts',(15.3893037522639,-9.78830977806044,10.0501174002428));
#14023=CARTESIAN_POINT('Ctrl Pts',(15.4578478923357,-9.84598388161831,10.0811552139138));
#14024=CARTESIAN_POINT('Ctrl Pts',(15.5263046465628,-9.90355602888934,10.1121249718658));
#14025=CARTESIAN_POINT('Ctrl Pts',(15.5946518761319,-9.96100982960575,10.1430193787867));
#14026=CARTESIAN_POINT('Ctrl Pts',(15.663218932117,-10.0186484200082,10.1740131519407));
#14027=CARTESIAN_POINT('Ctrl Pts',(15.7316757577788,-10.076167877539,10.2049310789385));
#14028=CARTESIAN_POINT('Ctrl Pts',(15.8,-10.1335518448686,10.2357659846983));
#14029=CARTESIAN_POINT('Origin',(15.8,0.,0.));
#14030=CARTESIAN_POINT('',(15.8,-12.8006061549939,6.60335220557564));
#14031=CARTESIAN_POINT('Ctrl Pts',(10.0502525316942,-7.28928030147641,5.55043285230422));
#14032=CARTESIAN_POINT('Ctrl Pts',(10.2399762236017,-7.47639594802579,5.59018769560147));
#14033=CARTESIAN_POINT('Ctrl Pts',(10.4321763653281,-7.66535745978524,5.62953666502922));
#14034=CARTESIAN_POINT('Ctrl Pts',(10.6261221631183,-7.85537951329499,5.66846318065078));
#14035=CARTESIAN_POINT('Ctrl Pts',(10.8155134734698,-8.04093922183172,5.70647557321088));
#14036=CARTESIAN_POINT('Ctrl Pts',(11.0065694150225,-8.2275101466569,5.74408496164242));
#14037=CARTESIAN_POINT('Ctrl Pts',(11.1986094788108,-8.41441083753267,5.78127435838123));
#14038=CARTESIAN_POINT('Ctrl Pts',(11.3896744033043,-8.60036248577474,5.81827491513844));
#14039=CARTESIAN_POINT('Ctrl Pts',(11.5817134810741,-8.78664049259051,5.854859475011));
#14040=CARTESIAN_POINT('Ctrl Pts',(11.774056517052,-8.972625000163,5.89101292727611));
#14041=CARTESIAN_POINT('Ctrl Pts',(11.9659982062652,-9.15822142880141,5.92709094103613));
#14042=CARTESIAN_POINT('Ctrl Pts',(12.1582425865196,-9.3435255923404,5.96273934048966));
#14043=CARTESIAN_POINT('Ctrl Pts',(12.3501236493256,-9.52797309682552,5.99794900016104));
#14044=CARTESIAN_POINT('Ctrl Pts',(12.5349923977935,-9.70567994717112,6.03187191898507));
#14045=CARTESIAN_POINT('Ctrl Pts',(12.7195238985377,-9.88259194572935,6.06538737998544));
#14046=CARTESIAN_POINT('Ctrl Pts',(12.9031225251803,-10.0582492231335,6.0984963351851));
#14047=CARTESIAN_POINT('Ctrl Pts',(13.0466099992771,-10.1955303101566,6.12437191191712));
#14048=CARTESIAN_POINT('Ctrl Pts',(13.1909144693232,-10.3333513349338,6.15023362158894));
#14049=CARTESIAN_POINT('Ctrl Pts',(13.3358225135832,-10.4715105676525,6.17605409599263));
#14050=CARTESIAN_POINT('Ctrl Pts',(13.4722456635829,-10.6015800736297,6.20036268749026));
#14051=CARTESIAN_POINT('Ctrl Pts',(13.6092037742271,-10.7319493881454,6.22463472522239));
#14052=CARTESIAN_POINT('Ctrl Pts',(13.7465187613193,-10.8624548834565,6.24884824365307));
#14053=CARTESIAN_POINT('Ctrl Pts',(13.8831227642785,-10.9922846525529,6.27293639028148));
#14054=CARTESIAN_POINT('Ctrl Pts',(14.0200799576114,-11.1222491940658,6.29696660630782));
#14055=CARTESIAN_POINT('Ctrl Pts',(14.1572150090555,-11.2521912379382,6.32091824773854));
#14056=CARTESIAN_POINT('Ctrl Pts',(14.4088957069996,-11.4906707801829,6.36487612552919));
#14057=CARTESIAN_POINT('Ctrl Pts',(14.6611754735305,-11.7290715847954,6.40856830116391));
#14058=CARTESIAN_POINT('Ctrl Pts',(14.9129704662266,-11.9664560266731,6.45187850892362));
#14059=CARTESIAN_POINT('Ctrl Pts',(14.9348533776089,-11.9870865509323,6.45564249735012));
#14060=CARTESIAN_POINT('Ctrl Pts',(14.9567326275237,-12.007709429512,6.45940361158509));
#14061=CARTESIAN_POINT('Ctrl Pts',(14.9786075045277,-12.0283240646364,6.46316178167156));
#14062=CARTESIAN_POINT('Ctrl Pts',(15.1157365203997,-12.1575528884896,6.48672096169998));
#14063=CARTESIAN_POINT('Ctrl Pts',(15.252693690801,-12.2864573923713,6.5101642983752));
#14064=CARTESIAN_POINT('Ctrl Pts',(15.3893037522639,-12.4148928744451,6.53347557107031));
#14065=CARTESIAN_POINT('Ctrl Pts',(15.4578478923357,-12.4793354168112,6.54517200926641));
#14066=CARTESIAN_POINT('Ctrl Pts',(15.5263046465628,-12.5436599631772,6.5568352285584));
#14067=CARTESIAN_POINT('Ctrl Pts',(15.5946518761319,-12.6078486707221,6.56846335549623));
#14068=CARTESIAN_POINT('Ctrl Pts',(15.663218932117,-12.6722438295541,6.58012888218654));
#14069=CARTESIAN_POINT('Ctrl Pts',(15.7316757577788,-12.7365022490344,6.59175908863286));
#14070=CARTESIAN_POINT('Ctrl Pts',(15.8,-12.8006061549939,6.60335220557564));
#14071=CARTESIAN_POINT('Origin',(15.8,0.,0.));
#14072=CARTESIAN_POINT('',(15.8,-14.2146479476009,2.32455630431103));
#14073=CARTESIAN_POINT('Ctrl Pts',(10.0502525316942,-8.64769560732005,3.02626384252387));
#14074=CARTESIAN_POINT('Ctrl Pts',(10.2399538592853,-8.83791565898925,3.00625338967612));
#14075=CARTESIAN_POINT('Ctrl Pts',(10.43213105289,-9.02976542249276,2.98528677263246));
#14076=CARTESIAN_POINT('Ctrl Pts',(10.6260535771573,-9.22249314018085,2.96359080496243));
#14077=CARTESIAN_POINT('Ctrl Pts',(10.8154434277105,-9.41071611112417,2.94240195085607));
#14078=CARTESIAN_POINT('Ctrl Pts',(11.0064979730137,-9.59977633037473,2.92051732350848));
#14079=CARTESIAN_POINT('Ctrl Pts',(11.198536715505,-9.78902046263172,2.89813133617979));
#14080=CARTESIAN_POINT('Ctrl Pts',(11.3896029988924,-9.97730628732604,2.8758587085664));
#14081=CARTESIAN_POINT('Ctrl Pts',(11.5816435370135,-10.1657740234644,2.85308955972929));
#14082=CARTESIAN_POINT('Ctrl Pts',(11.7739881178974,-10.3538294697532,2.8300010668165));
#14083=CARTESIAN_POINT('Ctrl Pts',(11.9659332365655,-10.5414943615229,2.80696052420466));
#14084=CARTESIAN_POINT('Ctrl Pts',(12.1581811364325,-10.7287485903519,2.78360167031412));
#14085=CARTESIAN_POINT('Ctrl Pts',(12.3500657725605,-10.9150525380997,2.76009024231665));
#14086=CARTESIAN_POINT('Ctrl Pts',(12.5349538836687,-11.0945634446848,2.73743609136625));
#14087=CARTESIAN_POINT('Ctrl Pts',(12.7195047388318,-11.2731923646042,2.71463999548716));
#14088=CARTESIAN_POINT('Ctrl Pts',(12.9031225251803,-11.4505020946774,2.69184501333336));
#14089=CARTESIAN_POINT('Ctrl Pts',(13.0466099992771,-11.5890601603578,2.67403195460754));
#14090=CARTESIAN_POINT('Ctrl Pts',(13.1909144693232,-11.7281274609627,2.65603885317597));
#14091=CARTESIAN_POINT('Ctrl Pts',(13.3358225135832,-11.8675036836248,2.63790201856914));
#14092=CARTESIAN_POINT('Ctrl Pts',(13.4722456635829,-11.9987189203477,2.62082716174719));
#14093=CARTESIAN_POINT('Ctrl Pts',(13.6092037742271,-12.1302080042448,2.60362489076148));
#14094=CARTESIAN_POINT('Ctrl Pts',(13.7465187613193,-12.2618085151784,2.58632488288814));
#14095=CARTESIAN_POINT('Ctrl Pts',(13.8831227642785,-12.3927276301685,2.56911445031434));
#14096=CARTESIAN_POINT('Ctrl Pts',(14.0200799576114,-12.5237570157981,2.55180727580019));
#14097=CARTESIAN_POINT('Ctrl Pts',(14.1572150090555,-12.6547407331994,2.53443232271127));
#14098=CARTESIAN_POINT('Ctrl Pts',(14.4088349682203,-12.895074019815,2.5025521801752));
#14099=CARTESIAN_POINT('Ctrl Pts',(14.6610537068573,-13.1352504185255,2.47044377568216));
#14100=CARTESIAN_POINT('Ctrl Pts',(14.912788167055,-13.3743428798791,2.43828616201247));
#14101=CARTESIAN_POINT('Ctrl Pts',(14.9347318651856,-13.3951845747076,2.43548298216013));
#14102=CARTESIAN_POINT('Ctrl Pts',(14.956671883472,-13.4160180659846,2.43267942911478));
#14103=CARTESIAN_POINT('Ctrl Pts',(14.9786075045277,-13.4368427586266,2.42987562206087));
#14104=CARTESIAN_POINT('Ctrl Pts',(15.1157365203996,-13.5670268824575,2.4123478164419));
#14105=CARTESIAN_POINT('Ctrl Pts',(15.252693690801,-13.6968667539964,2.39481006097156));
#14106=CARTESIAN_POINT('Ctrl Pts',(15.3893037522639,-13.8262197421006,2.3772916450855));
#14107=CARTESIAN_POINT('Ctrl Pts',(15.4578478923357,-13.8911226433977,2.368501774563));
#14108=CARTESIAN_POINT('Ctrl Pts',(15.5263046465628,-13.9559030572657,2.35971677469615));
#14109=CARTESIAN_POINT('Ctrl Pts',(15.5946518761319,-14.0205434363407,2.3509403772656));
#14110=CARTESIAN_POINT('Ctrl Pts',(15.663218932117,-14.085391719422,2.34213575215115));
#14111=CARTESIAN_POINT('Ctrl Pts',(15.7316757577788,-14.1500990399651,2.33333979124571));
#14112=CARTESIAN_POINT('Ctrl Pts',(15.8,-14.2146479476009,2.32455630431103));
#14113=CARTESIAN_POINT('Origin',(15.8,0.,0.));
#14114=CARTESIAN_POINT('Ctrl Pts',(10.0502525316942,9.2755658561365,-5.45537535466284));
#14115=CARTESIAN_POINT('Ctrl Pts',(11.1454425256572,10.527811485966,-5.54272139501844));
#14116=CARTESIAN_POINT('Ctrl Pts',(12.3775312688656,11.9365878195243,-5.64098569041847));
#14117=CARTESIAN_POINT('Ctrl Pts',(13.7465187613193,13.5018948568112,-5.75016824086296));
#14118=CARTESIAN_POINT('Ctrl Pts',(14.2941137583009,14.1280176717259,-5.79384126104075));
#14119=CARTESIAN_POINT('Ctrl Pts',(14.8417087552824,14.7541404866407,-5.83751428121855));
#14120=CARTESIAN_POINT('Ctrl Pts',(15.3208543776412,15.3019979496911,-5.87572817387412));
#14121=CARTESIAN_POINT('Ctrl Pts',(15.5946518761319,15.6150593571485,-5.89756468396302));
#14122=CARTESIAN_POINT('Ctrl Pts',(15.7315506253773,15.7715900608772,-5.90848293900747));
#14123=CARTESIAN_POINT('Ctrl Pts',(15.8,15.8498554127416,-5.91394206652969));
#14124=CARTESIAN_POINT('Ctrl Pts',(10.0502525316942,9.09326359699885,-5.66046875858054));
#14125=CARTESIAN_POINT('Ctrl Pts',(11.1454425256572,10.3398594101876,-5.77604676609018));
#14126=CARTESIAN_POINT('Ctrl Pts',(12.3775312688656,11.7423187718539,-5.90654052031257));
#14127=CARTESIAN_POINT('Ctrl Pts',(13.7465187613193,13.3005670731329,-6.05105541408884));
#14128=CARTESIAN_POINT('Ctrl Pts',(14.2941137583009,13.9238668895967,-6.10886731837785));
#14129=CARTESIAN_POINT('Ctrl Pts',(14.8417087552824,14.5471710567224,-6.16673138983645));
#14130=CARTESIAN_POINT('Ctrl Pts',(15.3208543776412,15.0925608480023,-6.21734620559882));
#14131=CARTESIAN_POINT('Ctrl Pts',(15.5946518761319,15.4042104768461,-6.24624880770452));
#14132=CARTESIAN_POINT('Ctrl Pts',(15.7315506253773,15.5600357233504,-6.26070528969669));
#14133=CARTESIAN_POINT('Ctrl Pts',(15.8,15.6379479616747,-6.26792891516604));
#14134=CARTESIAN_POINT('Ctrl Pts',(10.0502525316942,8.78255765938311,-5.94355560685308));
#14135=CARTESIAN_POINT('Ctrl Pts',(11.1454425256572,10.0148869038525,-6.10292787924083));
#14136=CARTESIAN_POINT('Ctrl Pts',(12.3775312688656,11.4012092316412,-6.28165449494742));
#14137=CARTESIAN_POINT('Ctrl Pts',(13.7465187613194,12.9416164381759,-6.48081852219946));
#14138=CARTESIAN_POINT('Ctrl Pts',(14.2941137583009,13.5577787105922,-6.56047693355266));
#14139=CARTESIAN_POINT('Ctrl Pts',(14.8417087552824,14.1739356301478,-6.64007218801817));
#14140=CARTESIAN_POINT('Ctrl Pts',(15.3208543776412,14.7130746018355,-6.70973770503941));
#14141=CARTESIAN_POINT('Ctrl Pts',(15.594651876132,15.0211560817903,-6.74957096648569));
#14142=CARTESIAN_POINT('Ctrl Pts',(15.7315506253773,15.1751962901528,-6.76948132483474));
#14143=CARTESIAN_POINT('Ctrl Pts',(15.8,15.2522168679322,-6.77944209185897));
#14144=CARTESIAN_POINT('Ctrl Pts',(10.0502525316942,8.52639512605652,-5.98584659003549));
#14145=CARTESIAN_POINT('Ctrl Pts',(11.1454425256572,9.73363772297167,-6.16614182963237));
#14146=CARTESIAN_POINT('Ctrl Pts',(12.3775312688656,11.0917875706281,-6.36925721416675));
#14147=CARTESIAN_POINT('Ctrl Pts',(13.7465187613193,12.6008409910269,-6.59465188812855));
#14148=CARTESIAN_POINT('Ctrl Pts',(14.2941137583008,13.2044623836355,-6.68481335297615));
#14149=CARTESIAN_POINT('Ctrl Pts',(14.8417087552823,13.8080839907189,-6.77500635669625));
#14150=CARTESIAN_POINT('Ctrl Pts',(15.3208543776412,14.3362528301216,-6.85391541259335));
#14151=CARTESIAN_POINT('Ctrl Pts',(15.5946518761319,14.6380635126529,-6.89899411967348));
#14152=CARTESIAN_POINT('Ctrl Pts',(15.7315506253773,14.7889688752189,-6.9215366054706));
#14153=CARTESIAN_POINT('Ctrl Pts',(15.8,14.8644215375261,-6.9328050579454));
#14154=CARTESIAN_POINT('Ctrl Pts',(10.0502525316942,8.35233000922534,-5.94770436886829));
#14155=CARTESIAN_POINT('Ctrl Pts',(11.1454425256572,9.5384055936255,-6.13452948592057));
#14156=CARTESIAN_POINT('Ctrl Pts',(12.3775312688656,10.8728200811769,-6.34492663085593));
#14157=CARTESIAN_POINT('Ctrl Pts',(13.7465187613193,12.3554217499083,-6.57847782979355));
#14158=CARTESIAN_POINT('Ctrl Pts',(14.2941137583008,12.9484634259519,-6.67190108779269));
#14159=CARTESIAN_POINT('Ctrl Pts',(14.8417087552824,13.541513949349,-6.7653487190758));
#14160=CARTESIAN_POINT('Ctrl Pts',(15.3208543776412,14.0604304019321,-6.84710780571678));
#14161=CARTESIAN_POINT('Ctrl Pts',(15.5946518761319,14.3569506718,-6.89381786952799));
#14162=CARTESIAN_POINT('Ctrl Pts',(15.7315506253773,14.5052116854016,-6.91717532204614));
#14163=CARTESIAN_POINT('Ctrl Pts',(15.8,14.5793414094266,-6.92885189186191));
#14164=CARTESIAN_POINT('Ctrl Pts',(10.0502525316942,8.1751443698686,-5.91814205125966));
#14165=CARTESIAN_POINT('Ctrl Pts',(11.1454425256572,9.34066488658195,-6.11093026523681));
#14166=CARTESIAN_POINT('Ctrl Pts',(12.3775312688656,10.6518240329443,-6.32804641946555));
#14167=CARTESIAN_POINT('Ctrl Pts',(13.7465187613193,12.1087200255634,-6.56905244176937));
#14168=CARTESIAN_POINT('Ctrl Pts',(14.2941137583008,12.6914777697296,-6.66545776271566));
#14169=CARTESIAN_POINT('Ctrl Pts',(14.8417087552823,13.2742297865971,-6.76188862893654));
#14170=CARTESIAN_POINT('Ctrl Pts',(15.3208543776412,13.7841395850464,-6.84625768114734));
#14171=CARTESIAN_POINT('Ctrl Pts',(15.5946518761319,14.0755188249216,-6.89445870116996));
#14172=CARTESIAN_POINT('Ctrl Pts',(15.7315506253773,14.2212078760573,-6.91856174818909));
#14173=CARTESIAN_POINT('Ctrl Pts',(15.8,14.2940529083518,-6.93061101156266));
#14174=CARTESIAN_POINT('Ctrl Pts',(10.0502525316942,7.90144264462466,-5.89433124999989));
#14175=CARTESIAN_POINT('Ctrl Pts',(11.1454425256572,9.03654403267794,-6.09882926548583));
#14176=CARTESIAN_POINT('Ctrl Pts',(12.3775312688656,10.3136205759385,-6.32895925304844));
#14177=CARTESIAN_POINT('Ctrl Pts',(13.7465187613193,11.7325052253954,-6.58458807992399));
#14178=CARTESIAN_POINT('Ctrl Pts',(14.2941137583008,12.3000601956136,-6.68684049565602));
#14179=CARTESIAN_POINT('Ctrl Pts',(14.8417087552823,12.86762490695,-6.78910067475031));
#14180=CARTESIAN_POINT('Ctrl Pts',(15.3208543776411,13.364240995629,-6.87857591366297));
#14181=CARTESIAN_POINT('Ctrl Pts',(15.5946518761319,13.6480178551891,-6.92970162298622));
#14182=CARTESIAN_POINT('Ctrl Pts',(15.7315506253773,13.7899072524002,-6.95526524865976));
#14183=CARTESIAN_POINT('Ctrl Pts',(15.8,13.8608510891535,-6.96804637462763));
#14184=CARTESIAN_POINT('Ctrl Pts',(10.0502525316942,7.66237562613099,-5.80163007173557));
#14185=CARTESIAN_POINT('Ctrl Pts',(11.1454425256572,8.76621669669801,-6.00977287125004));
#14186=CARTESIAN_POINT('Ctrl Pts',(12.3775312688656,10.008064757174,-6.24400287259235));
#14187=CARTESIAN_POINT('Ctrl Pts',(13.7465187613193,11.3878685250288,-6.50418764618811));
#14188=CARTESIAN_POINT('Ctrl Pts',(14.2941137583008,11.9397903730643,-6.60826243593386));
#14189=CARTESIAN_POINT('Ctrl Pts',(14.8417087552823,12.4917152115347,-6.71234494803684));
#14190=CARTESIAN_POINT('Ctrl Pts',(15.3208543776411,12.9746485138656,-6.80341474110257));
#14191=CARTESIAN_POINT('Ctrl Pts',(15.5946518761319,13.2506092458454,-6.85545164006593));
#14192=CARTESIAN_POINT('Ctrl Pts',(15.7315506253773,13.388589908828,-6.88147085648712));
#14193=CARTESIAN_POINT('Ctrl Pts',(15.8,13.4575799757384,-6.89447978145678));
#14194=CARTESIAN_POINT('Ctrl Pts',(10.0502525316942,7.44593237535689,-5.68351040711503));
#14195=CARTESIAN_POINT('Ctrl Pts',(11.1454425256572,8.51992624992032,-5.89012315163303));
#14196=CARTESIAN_POINT('Ctrl Pts',(12.3775312688656,9.72815762348205,-6.12263633930509));
#14197=CARTESIAN_POINT('Ctrl Pts',(13.7465187613194,11.0706489050023,-6.38090895110342));
#14198=CARTESIAN_POINT('Ctrl Pts',(14.2941137583009,11.60764526865,-6.48421893322741));
#14199=CARTESIAN_POINT('Ctrl Pts',(14.8417087552824,12.1446403255654,-6.58753713858488));
#14200=CARTESIAN_POINT('Ctrl Pts',(15.3208543776412,12.6145114073305,-6.67793800725711));
#14201=CARTESIAN_POINT('Ctrl Pts',(15.594651876132,12.8830096730692,-6.72959247024462));
#14202=CARTESIAN_POINT('Ctrl Pts',(15.7315506253773,13.0172586761616,-6.75542051842202));
#14203=CARTESIAN_POINT('Ctrl Pts',(15.8,13.0843832933218,-6.76833381495439));
#14204=CARTESIAN_POINT('Ctrl Pts',(10.0502525316942,7.34913449516209,-5.60747221894231));
#14205=CARTESIAN_POINT('Ctrl Pts',(11.1454425256572,8.40845336995523,-5.81105284226644));
#14206=CARTESIAN_POINT('Ctrl Pts',(12.3775312688656,9.60029668798142,-6.04008639989119));
#14207=CARTESIAN_POINT('Ctrl Pts',(13.7465187613193,10.9244551954278,-6.29456266363367));
#14208=CARTESIAN_POINT('Ctrl Pts',(14.2941137583009,11.4541199893924,-6.39635323712111));
#14209=CARTESIAN_POINT('Ctrl Pts',(14.8417087552824,11.9837969855611,-6.49814440704392));
#14210=CARTESIAN_POINT('Ctrl Pts',(15.3208543776412,12.4472605569962,-6.58721149497459));
#14211=CARTESIAN_POINT('Ctrl Pts',(15.5946518761319,12.7120921703849,-6.6381067434168));
#14212=CARTESIAN_POINT('Ctrl Pts',(15.7315506253773,12.8445091889311,-6.66355442687239));
#14213=CARTESIAN_POINT('Ctrl Pts',(15.8,12.9107166186057,-6.67627821583014));
#14214=CARTESIAN_POINT('Ctrl Pts',(10.0502525316942,7.28928030147641,-5.55043285230422));
#14215=CARTESIAN_POINT('Ctrl Pts',(11.1454425256572,8.33905665452735,-5.75098891959401));
#14216=CARTESIAN_POINT('Ctrl Pts',(12.3775312688656,9.52005505170966,-5.97661449529503));
#14217=CARTESIAN_POINT('Ctrl Pts',(13.7465187613193,10.8322754930233,-6.22730957940728));
#14218=CARTESIAN_POINT('Ctrl Pts',(14.2941137583009,11.3571636695488,-6.32758761305217));
#14219=CARTESIAN_POINT('Ctrl Pts',(14.8417087552824,11.8820518460743,-6.42786564669707));
#14220=CARTESIAN_POINT('Ctrl Pts',(15.3208543776412,12.3413290005341,-6.51560892613635));
#14221=CARTESIAN_POINT('Ctrl Pts',(15.5946518761319,12.6037730887968,-6.56574794295881));
#14222=CARTESIAN_POINT('Ctrl Pts',(15.7315506253773,12.7349951329282,-6.59081745137003));
#14223=CARTESIAN_POINT('Ctrl Pts',(15.8,12.8006061549939,-6.60335220557564));
#14224=CARTESIAN_POINT('Ctrl Pts',(15.8,12.8370600702028,-6.62691983743441));
#14225=CARTESIAN_POINT('Ctrl Pts',(15.8,12.8297280642598,-6.62229417791417));
#14226=CARTESIAN_POINT('Ctrl Pts',(15.8,12.8224166748639,-6.61762457479065));
#14227=CARTESIAN_POINT('Ctrl Pts',(15.8,12.8151258955788,-6.6129110406524));
#14228=CARTESIAN_POINT('Ctrl Pts',(15.8,12.8078557223109,-6.60815358414732));
#14229=CARTESIAN_POINT('Ctrl Pts',(15.8,12.8006061549939,-6.60335220557564));
#14230=CARTESIAN_POINT('Origin',(15.8,13.950492764499,-5.67212567669951));
#14231=CARTESIAN_POINT('Ctrl Pts',(10.0502525316942,7.13578365451837,-8.05467776187827));
#14232=CARTESIAN_POINT('Ctrl Pts',(11.1454425256572,8.29974860990864,-8.52471396348012));
#14233=CARTESIAN_POINT('Ctrl Pts',(12.3775312688656,9.6092091847227,-9.05350469028219));
#14234=CARTESIAN_POINT('Ctrl Pts',(13.7465187613193,11.0641653789605,-9.6410499422845));
#14235=CARTESIAN_POINT('Ctrl Pts',(14.2941137583009,11.6461478566557,-9.87606804308543));
#14236=CARTESIAN_POINT('Ctrl Pts',(14.8417087552824,12.2281303343508,-10.1110861438864));
#14237=CARTESIAN_POINT('Ctrl Pts',(15.3208543776412,12.737365002334,-10.3167269820872));
#14238=CARTESIAN_POINT('Ctrl Pts',(15.5946518761319,13.0283562411816,-10.4342360324876));
#14239=CARTESIAN_POINT('Ctrl Pts',(15.7315506253773,13.1738518606054,-10.4929905576879));
#14240=CARTESIAN_POINT('Ctrl Pts',(15.8,13.2465996703173,-10.522367820288));
#14241=CARTESIAN_POINT('Ctrl Pts',(10.0502525316942,6.89902655578542,-8.19339868393687));
#14242=CARTESIAN_POINT('Ctrl Pts',(11.1454425256572,8.04889405860838,-8.68853919251131));
#14243=CARTESIAN_POINT('Ctrl Pts',(12.3775312688656,9.34238794408146,-9.24602752966092));
#14244=CARTESIAN_POINT('Ctrl Pts',(13.7465187613193,10.779712402918,-9.86499535005157));
#14245=CARTESIAN_POINT('Ctrl Pts',(14.2941137583009,11.354640872798,-10.1125880646808));
#14246=CARTESIAN_POINT('Ctrl Pts',(14.8417087552824,11.9295571981554,-10.3602324253388));
#14247=CARTESIAN_POINT('Ctrl Pts',(15.3208543776412,12.4326127553978,-10.5769051976768));
#14248=CARTESIAN_POINT('Ctrl Pts',(15.5946518761319,12.7200777462785,-10.7006983402633));
#14249=CARTESIAN_POINT('Ctrl Pts',(15.7315506253773,12.8638090371883,-10.7626000339661));
#14250=CARTESIAN_POINT('Ctrl Pts',(15.8,12.9356757561148,-10.793546315752));
#14251=CARTESIAN_POINT('Ctrl Pts',(10.0502525316942,6.51604789180995,-8.36661813687799));
#14252=CARTESIAN_POINT('Ctrl Pts',(11.1454425256572,7.63881390938369,-8.89900085425541));
#14253=CARTESIAN_POINT('Ctrl Pts',(12.3775312688656,8.90205445633837,-9.49738068383037));
#14254=CARTESIAN_POINT('Ctrl Pts',(13.7465187613194,10.3055239107478,-10.1628080503653));
#14255=CARTESIAN_POINT('Ctrl Pts',(14.2941137583009,10.8669132727126,-10.4289722391039));
#14256=CARTESIAN_POINT('Ctrl Pts',(14.8417087552824,11.4283172433782,-10.6950739523901));
#14257=CARTESIAN_POINT('Ctrl Pts',(15.3208543776412,11.9195411796877,-10.9279323587878));
#14258=CARTESIAN_POINT('Ctrl Pts',(15.5946518761319,12.2002349513456,-11.061018341967));
#14259=CARTESIAN_POINT('Ctrl Pts',(15.7315506253773,12.3405832861097,-11.1275551370521));
#14260=CARTESIAN_POINT('Ctrl Pts',(15.8,12.4107561622081,-11.1608290568882));
#14261=CARTESIAN_POINT('Ctrl Pts',(10.0502525316942,6.25935291859363,-8.32768215464935));
#14262=CARTESIAN_POINT('Ctrl Pts',(11.1454425256572,7.35179456409853,-8.87221159590509));
#14263=CARTESIAN_POINT('Ctrl Pts',(12.3775312688656,8.5807059309797,-9.48507728715609));
#14264=CARTESIAN_POINT('Ctrl Pts',(13.7465187613193,9.94625006691878,-10.1657641132886));
#14265=CARTESIAN_POINT('Ctrl Pts',(14.2941137583008,10.4924666723322,-10.4380421577189));
#14266=CARTESIAN_POINT('Ctrl Pts',(14.8417087552823,11.0386735802612,-10.7103508393265));
#14267=CARTESIAN_POINT('Ctrl Pts',(15.3208543776411,11.5166076371098,-10.9486114186505));
#14268=CARTESIAN_POINT('Ctrl Pts',(15.5946518761319,11.7897165434404,-11.0847485338421));
#14269=CARTESIAN_POINT('Ctrl Pts',(15.7315506253773,11.9262700347798,-11.1528201301259));
#14270=CARTESIAN_POINT('Ctrl Pts',(15.8,11.9945476376239,-11.1868532202044));
#14271=CARTESIAN_POINT('Ctrl Pts',(10.0502525316942,6.10559301495173,-8.23761851725688));
#14272=CARTESIAN_POINT('Ctrl Pts',(11.1454425256572,7.17588579216884,-8.7818172744299));
#14273=CARTESIAN_POINT('Ctrl Pts',(12.3775312688656,8.37997276877533,-9.39427431712614));
#14274=CARTESIAN_POINT('Ctrl Pts',(13.7465187613193,9.71783944471698,-10.0745443941304));
#14275=CARTESIAN_POINT('Ctrl Pts',(14.2941137583008,10.2529862083793,-10.3466552894421));
#14276=CARTESIAN_POINT('Ctrl Pts',(14.8417087552823,10.7881338344522,-10.61879266668));
#14277=CARTESIAN_POINT('Ctrl Pts',(15.3208543776412,11.2563877393682,-10.856904645461));
#14278=CARTESIAN_POINT('Ctrl Pts',(15.5946518761319,11.5239610675182,-10.9929584447386));
#14279=CARTESIAN_POINT('Ctrl Pts',(15.7315506253773,11.6577478171298,-11.060987970935));
#14280=CARTESIAN_POINT('Ctrl Pts',(15.8,11.7246411157058,-11.0950003932583));
#14281=CARTESIAN_POINT('Ctrl Pts',(10.0502525316941,5.94621492062452,-8.15474945546092));
#14282=CARTESIAN_POINT('Ctrl Pts',(11.1454425256572,6.99511596848632,-8.69826758958589));
#14283=CARTESIAN_POINT('Ctrl Pts',(12.3775312688656,8.17501015002258,-9.30992859260386));
#14284=CARTESIAN_POINT('Ctrl Pts',(13.7465187613193,9.48612538727717,-9.98934507962172));
#14285=CARTESIAN_POINT('Ctrl Pts',(14.2941137583008,10.0105700158496,-10.2611141666576));
#14286=CARTESIAN_POINT('Ctrl Pts',(14.8417087552823,10.535001088446,-10.532906293941));
#14287=CARTESIAN_POINT('Ctrl Pts',(15.3208543776412,10.9938824879741,-10.7707172481292));
#14288=CARTESIAN_POINT('Ctrl Pts',(15.5946518761319,11.2561056460575,-10.9066003574976));
#14289=CARTESIAN_POINT('Ctrl Pts',(15.7315506253773,11.3872158805765,-10.9745441973833));
#14290=CARTESIAN_POINT('Ctrl Pts',(15.8,11.4527721960679,-11.0085140807661));
#14291=CARTESIAN_POINT('Ctrl Pts',(10.0502525316942,5.69326714724857,-8.04752551167496));
#14292=CARTESIAN_POINT('Ctrl Pts',(11.1454425256572,6.70961935691121,-8.59278030111934));
#14293=CARTESIAN_POINT('Ctrl Pts',(12.3775312688656,7.85307681747464,-9.20628631668584));
#14294=CARTESIAN_POINT('Ctrl Pts',(13.7465187613193,9.12352275260843,-9.8878635484672));
#14295=CARTESIAN_POINT('Ctrl Pts',(14.2941137583008,9.63170187793886,-10.1604955992679));
#14296=CARTESIAN_POINT('Ctrl Pts',(14.8417087552823,10.1398879487016,-10.4331383564046));
#14297=CARTESIAN_POINT('Ctrl Pts',(15.3208543776412,10.5845486031013,-10.6716974431005));
#14298=CARTESIAN_POINT('Ctrl Pts',(15.5946518761319,10.8386377334452,-10.8080128020807));
#14299=CARTESIAN_POINT('Ctrl Pts',(15.7315506253773,10.9656829874862,-10.8761715434576));
#14300=CARTESIAN_POINT('Ctrl Pts',(15.8,11.0292050005901,-10.9102499677978));
#14301=CARTESIAN_POINT('Ctrl Pts',(10.0502525316942,5.49454791241252,-7.88548479029561));
#14302=CARTESIAN_POINT('Ctrl Pts',(11.1454425256572,6.48004349322276,-8.42454600598801));
#14303=CARTESIAN_POINT('Ctrl Pts',(12.3775312688655,7.5887300381936,-9.03106484753221));
#14304=CARTESIAN_POINT('Ctrl Pts',(13.7465187613193,8.82059988637917,-9.70489831419831));
#14305=CARTESIAN_POINT('Ctrl Pts',(14.2941137583008,9.31334787493986,-9.97443262085553));
#14306=CARTESIAN_POINT('Ctrl Pts',(14.8417087552823,9.8060963191458,-10.2439754326772));
#14307=CARTESIAN_POINT('Ctrl Pts',(15.3208543776411,10.2372510662851,-10.4798227509907));
#14308=CARTESIAN_POINT('Ctrl Pts',(15.5946518761319,10.4836250322036,-10.6145893749119));
#14309=CARTESIAN_POINT('Ctrl Pts',(15.7315506253773,10.6068120603552,-10.6819735304405));
#14310=CARTESIAN_POINT('Ctrl Pts',(15.8,10.6684055341558,-10.7156648564213));
#14311=CARTESIAN_POINT('Ctrl Pts',(10.0502525316942,5.32519947010607,-7.70626127860212));
#14312=CARTESIAN_POINT('Ctrl Pts',(11.1454425256572,6.28278149366019,-8.23464403472028));
#14313=CARTESIAN_POINT('Ctrl Pts',(12.3775312688656,7.3600274050152,-8.82914182271549));
#14314=CARTESIAN_POINT('Ctrl Pts',(13.7465187613194,8.55700179652725,-9.48962649341722));
#14315=CARTESIAN_POINT('Ctrl Pts',(14.2941137583009,9.03579113757914,-9.75382118614166));
#14316=CARTESIAN_POINT('Ctrl Pts',(14.8417087552824,9.51457663691211,-10.0180235007136));
#14317=CARTESIAN_POINT('Ctrl Pts',(15.3208543776412,9.93351514221374,-10.2491981583259));
#14318=CARTESIAN_POINT('Ctrl Pts',(15.594651876132,10.172910051869,-10.3812950302631));
#14319=CARTESIAN_POINT('Ctrl Pts',(15.7315506253773,10.2926071256634,-10.4473442221896));
#14320=CARTESIAN_POINT('Ctrl Pts',(15.8,10.3524560021355,-10.480368144447));
#14321=CARTESIAN_POINT('Ctrl Pts',(10.0502525316942,5.25663803961482,-7.60403044672135));
#14322=CARTESIAN_POINT('Ctrl Pts',(11.1454425256572,6.20120028598869,-8.12499465989843));
#14323=CARTESIAN_POINT('Ctrl Pts',(12.3775312688656,7.2639348461738,-8.71111815506916));
#14324=CARTESIAN_POINT('Ctrl Pts',(13.7465187613193,8.44464710847933,-9.36232701259537));
#14325=CARTESIAN_POINT('Ctrl Pts',(14.2941137583009,8.91693326542986,-9.62281103116557));
#14326=CARTESIAN_POINT('Ctrl Pts',(14.8417087552824,9.38923099717743,-9.88329944620756));
#14327=CARTESIAN_POINT('Ctrl Pts',(15.3208543776412,9.80248791688054,-10.1112254436565));
#14328=CARTESIAN_POINT('Ctrl Pts',(15.5946518761319,10.0386302748779,-10.2414671792814));
#14329=CARTESIAN_POINT('Ctrl Pts',(15.7315506253773,10.1567026018999,-10.3065884831493));
#14330=CARTESIAN_POINT('Ctrl Pts',(15.8,10.2157377422983,-10.3391487464728));
#14331=CARTESIAN_POINT('Ctrl Pts',(10.0502525316942,5.21733945232202,-7.53128682236137));
#14332=CARTESIAN_POINT('Ctrl Pts',(11.1454425256572,6.15376086042613,-8.04642571042556));
#14333=CARTESIAN_POINT('Ctrl Pts',(12.3775312688656,7.20723494454326,-8.62595695949777));
#14334=CARTESIAN_POINT('Ctrl Pts',(13.7465187613193,8.37776170467339,-9.269880569578));
#14335=CARTESIAN_POINT('Ctrl Pts',(14.2941137583009,8.84597240872545,-9.52745001361009));
#14336=CARTESIAN_POINT('Ctrl Pts',(14.8417087552824,9.31418311277751,-9.78501945764219));
#14337=CARTESIAN_POINT('Ctrl Pts',(15.3208543776412,9.72386747882305,-10.0103927211703));
#14338=CARTESIAN_POINT('Ctrl Pts',(15.5946518761319,9.95797283084908,-10.1391774431863));
#14339=CARTESIAN_POINT('Ctrl Pts',(15.7315506253773,10.0750255068621,-10.2035698041943));
#14340=CARTESIAN_POINT('Ctrl Pts',(15.8,10.1335518448686,-10.2357659846983));
#14341=CARTESIAN_POINT('Ctrl Pts',(15.8,10.160938779711,-10.2694450138623));
#14342=CARTESIAN_POINT('Ctrl Pts',(15.8,10.1553950350833,-10.2627800357942));
#14343=CARTESIAN_POINT('Ctrl Pts',(15.8,10.1498844772774,-10.2560796357392));
#14344=CARTESIAN_POINT('Ctrl Pts',(15.8,10.1444070962816,-10.2493438236809));
#14345=CARTESIAN_POINT('Ctrl Pts',(15.8,10.1389628855307,-10.242572606579));
#14346=CARTESIAN_POINT('Ctrl Pts',(15.8,10.1335518448686,-10.2357659846983));
#14347=CARTESIAN_POINT('Origin',(15.8,11.5149238208745,-9.70545143020505));
#14348=CARTESIAN_POINT('Ctrl Pts',(10.0502525316942,4.29750123086779,-9.86553218952114));
#14349=CARTESIAN_POINT('Ctrl Pts',(11.9668350211294,5.98055897313701,-11.2772850923971));
#14350=CARTESIAN_POINT('Ctrl Pts',(13.8834175105647,7.66361671540623,-12.689037995273));
#14351=CARTESIAN_POINT('Ctrl Pts',(15.8,9.34667445767544,-14.1007908981489));
#14352=CARTESIAN_POINT('Ctrl Pts',(10.0502525316942,4.02946472694721,-9.92430165934404));
#14353=CARTESIAN_POINT('Ctrl Pts',(11.9668350211294,5.67542688932036,-11.3702854403574));
#14354=CARTESIAN_POINT('Ctrl Pts',(13.8834175105647,7.32120731702057,-12.8166324188796));
#14355=CARTESIAN_POINT('Ctrl Pts',(15.8,8.96716947939372,-14.262616199893));
#14356=CARTESIAN_POINT('Ctrl Pts',(10.0502525316942,3.61211062987325,-9.97045860619056));
#14357=CARTESIAN_POINT('Ctrl Pts',(11.9668350211294,5.19299729643613,-11.4635526451079));
#14358=CARTESIAN_POINT('Ctrl Pts',(13.8834175105647,6.77411605990066,-12.956112555571));
#14359=CARTESIAN_POINT('Ctrl Pts',(15.8,8.35500272646353,-14.4492065944883));
#14360=CARTESIAN_POINT('Ctrl Pts',(10.0502525316942,3.40259706500423,-9.86609404202409));
#14361=CARTESIAN_POINT('Ctrl Pts',(11.9668350211294,4.93192196434906,-11.3629139742223));
#14362=CARTESIAN_POINT('Ctrl Pts',(13.8834175105647,6.4612970474202,-12.8596985741914));
#14363=CARTESIAN_POINT('Ctrl Pts',(15.8,7.99062194676503,-14.3565185063896));
#14364=CARTESIAN_POINT('Ctrl Pts',(10.0502525316942,3.30601090928165,-9.77087387154055));
#14365=CARTESIAN_POINT('Ctrl Pts',(11.9668350211295,4.80688444200921,-11.2600017151873));
#14366=CARTESIAN_POINT('Ctrl Pts',(13.8834175105647,6.30755492143113,-12.7494883087275));
#14367=CARTESIAN_POINT('Ctrl Pts',(15.8,7.8084284541587,-14.2386161523742));
#14368=CARTESIAN_POINT('Ctrl Pts',(10.0502525316942,3.24522078037662,-9.7053049496755));
#14369=CARTESIAN_POINT('Ctrl Pts',(11.9668350211294,4.72781700580773,-11.1883166806211));
#14370=CARTESIAN_POINT('Ctrl Pts',(13.8834175105647,6.21037804061049,-12.6715703878316));
#14371=CARTESIAN_POINT('Ctrl Pts',(15.8,7.69297426604161,-14.1545821187772));
#14372=CARTESIAN_POINT('Ctrl Pts',(10.0502525316942,3.13558852137588,-9.59290229251195));
#14373=CARTESIAN_POINT('Ctrl Pts',(11.9668350211294,4.58744122478927,-11.0646742694967));
#14374=CARTESIAN_POINT('Ctrl Pts',(13.8834175105647,6.03905717649217,-12.5366026187688));
#14375=CARTESIAN_POINT('Ctrl Pts',(15.8,7.49090987990556,-14.0083745957535));
#14376=CARTESIAN_POINT('Ctrl Pts',(10.0502525316942,2.92757116168118,-9.41310152025599));
#14377=CARTESIAN_POINT('Ctrl Pts',(11.9668350211294,4.32424671627921,-10.8702564567215));
#14378=CARTESIAN_POINT('Ctrl Pts',(13.8834175105647,5.72097159497831,-12.3275956094625));
#14379=CARTESIAN_POINT('Ctrl Pts',(15.8,7.11764714957634,-13.784750545928));
#14380=CARTESIAN_POINT('Ctrl Pts',(10.0502525316942,2.78894862571458,-9.19740926566327));
#14381=CARTESIAN_POINT('Ctrl Pts',(11.9668350211294,4.13765656795513,-10.6275127538178));
#14382=CARTESIAN_POINT('Ctrl Pts',(13.8834175105647,5.48632659127461,-12.0577280234799));
#14383=CARTESIAN_POINT('Ctrl Pts',(15.8,6.83503453351516,-13.4878315116344));
#14384=CARTESIAN_POINT('Ctrl Pts',(10.0502525316942,2.68315129602989,-8.97469639188219));
#14385=CARTESIAN_POINT('Ctrl Pts',(11.9668350211294,3.99115284441713,-10.3719655284903));
#14386=CARTESIAN_POINT('Ctrl Pts',(13.8834175105647,5.29909475352164,-11.7692966119437));
#14387=CARTESIAN_POINT('Ctrl Pts',(15.8,6.60709630190888,-13.1665657485518));
#14388=CARTESIAN_POINT('Ctrl Pts',(10.0502525316942,2.64958522759923,-8.85625319397989));
#14389=CARTESIAN_POINT('Ctrl Pts',(11.9668350211294,3.93994688562079,-10.2341088589535));
#14390=CARTESIAN_POINT('Ctrl Pts',(13.8834175105647,5.23040962052304,-11.612095695752));
#14391=CARTESIAN_POINT('Ctrl Pts',(15.8,6.5207712785446,-12.9899513607256));
#14392=CARTESIAN_POINT('Ctrl Pts',(10.0502525316942,2.63468906623289,-8.77492596468499));
#14393=CARTESIAN_POINT('Ctrl Pts',(11.9668350211294,3.91464433600868,-10.1386945339445));
#14394=CARTESIAN_POINT('Ctrl Pts',(13.8834175105647,5.19459960578446,-11.5024631032041));
#14395=CARTESIAN_POINT('Ctrl Pts',(15.8,6.47455487556025,-12.8662316724636));
#14396=CARTESIAN_POINT('Ctrl Pts',(15.8,6.49019400603777,-12.9067253609027));
#14397=CARTESIAN_POINT('Ctrl Pts',(15.8,6.48698118307512,-12.8986734787776));
#14398=CARTESIAN_POINT('Ctrl Pts',(15.8,6.48381086865141,-12.890598163633));
#14399=CARTESIAN_POINT('Ctrl Pts',(15.8,6.48068305016014,-12.8824994218701));
#14400=CARTESIAN_POINT('Ctrl Pts',(15.8,6.47759771920651,-12.874377258079));
#14401=CARTESIAN_POINT('Ctrl Pts',(15.8,6.47455487556025,-12.8662316724636));
#14402=CARTESIAN_POINT('Origin',(15.8,7.95219390447097,-12.7887399758658));
#14403=CARTESIAN_POINT('Ctrl Pts',(10.0502525316942,1.03854944428814,-10.7106795892491));
#14404=CARTESIAN_POINT('Ctrl Pts',(11.9668350211294,2.20297683852746,-12.5734298318033));
#14405=CARTESIAN_POINT('Ctrl Pts',(13.8834175105647,3.36740423276678,-14.4361800743576));
#14406=CARTESIAN_POINT('Ctrl Pts',(15.8,4.5318316270061,-16.2989303169119));
#14407=CARTESIAN_POINT('Ctrl Pts',(10.0502525316942,0.765470815703813,-10.6837448416591));
#14408=CARTESIAN_POINT('Ctrl Pts',(11.9668350211294,1.88404029388038,-12.5675874193204));
#14409=CARTESIAN_POINT('Ctrl Pts',(13.8834175105647,3.00232469790949,-14.4517192592367));
#14410=CARTESIAN_POINT('Ctrl Pts',(15.8,4.12089417608606,-16.335561836898));
#14411=CARTESIAN_POINT('Ctrl Pts',(10.0502525316942,0.354275884655604,-10.5986742216641));
#14412=CARTESIAN_POINT('Ctrl Pts',(11.9668350211294,1.39639701818897,-12.5072118829665));
#14413=CARTESIAN_POINT('Ctrl Pts',(13.8834175105647,2.43890221878171,-14.4153151096236));
#14414=CARTESIAN_POINT('Ctrl Pts',(15.8,3.48102335231507,-16.3238527709261));
#14415=CARTESIAN_POINT('Ctrl Pts',(10.0502525316942,0.187261072828497,-10.4346757823309));
#14416=CARTESIAN_POINT('Ctrl Pts',(11.9668350211294,1.17919268731442,-12.3308235163868));
#14417=CARTESIAN_POINT('Ctrl Pts',(13.8834175105647,2.17117887432506,-14.2269575174279));
#14418=CARTESIAN_POINT('Ctrl Pts',(15.8,3.16311048881099,-16.1231052514838));
#14419=CARTESIAN_POINT('Ctrl Pts',(10.0502525316942,0.124824203483031,-10.3142698682631));
#14420=CARTESIAN_POINT('Ctrl Pts',(11.9668350211295,1.09207394643473,-12.1943100355803));
#14421=CARTESIAN_POINT('Ctrl Pts',(13.8834175105647,2.05901454824881,-14.0746341437949));
#14422=CARTESIAN_POINT('Ctrl Pts',(15.8,3.02626429120051,-15.9546743111121));
#14423=CARTESIAN_POINT('Ctrl Pts',(10.0502525316942,0.0872711810328548,
-10.2331249635989));
#14424=CARTESIAN_POINT('Ctrl Pts',(11.9668350211294,1.03902815454411,-12.1017003635113));
#14425=CARTESIAN_POINT('Ctrl Pts',(13.8834175105647,1.99067177195527,-13.9705005205662));
#14426=CARTESIAN_POINT('Ctrl Pts',(15.8,2.94242874546653,-15.8390759204785));
#14427=CARTESIAN_POINT('Ctrl Pts',(10.0502525316942,0.0177390798696538,
-10.09234540735));
#14428=CARTESIAN_POINT('Ctrl Pts',(11.9668350211294,0.943730501418605,-11.9407308952458));
#14429=CARTESIAN_POINT('Ctrl Pts',(13.8834175105647,1.86944300220408,-13.789197555515));
#14430=CARTESIAN_POINT('Ctrl Pts',(15.8,2.79543442375303,-15.6375830434108));
#14431=CARTESIAN_POINT('Ctrl Pts',(10.0502525316942,-0.124535428292434,
-9.85706386916291));
#14432=CARTESIAN_POINT('Ctrl Pts',(11.9668350211294,0.753496320252983,-11.6744970487389));
#14433=CARTESIAN_POINT('Ctrl Pts',(13.8834175105647,1.63151416409049,-13.4921256030567));
#14434=CARTESIAN_POINT('Ctrl Pts',(15.8,2.50954591263591,-15.3095587826327));
#14435=CARTESIAN_POINT('Ctrl Pts',(10.0502525316942,-0.189717758784556,
-9.60909091476054));
#14436=CARTESIAN_POINT('Ctrl Pts',(11.9668350211294,0.651053436707715,-11.3859738307471));
#14437=CARTESIAN_POINT('Ctrl Pts',(13.8834175105647,1.49175101418763,-13.1629551482145));
#14438=CARTESIAN_POINT('Ctrl Pts',(15.8,2.3325222096799,-14.9398380642011));
#14439=CARTESIAN_POINT('Ctrl Pts',(10.0502525316942,-0.221513186022214,
-9.36458479377687));
#14440=CARTESIAN_POINT('Ctrl Pts',(11.9668350211294,0.590690300968106,-11.0976614182865));
#14441=CARTESIAN_POINT('Ctrl Pts',(13.8834175105648,1.40281548080797,-12.8307816497324));
#14442=CARTESIAN_POINT('Ctrl Pts',(15.8,2.21501896779829,-14.563858274242));
#14443=CARTESIAN_POINT('Ctrl Pts',(10.0502525316942,-0.216827447239561,
-9.24156417346731));
#14444=CARTESIAN_POINT('Ctrl Pts',(11.9668350211294,0.58459859972662,-10.9507264633732));
#14445=CARTESIAN_POINT('Ctrl Pts',(13.8834175105647,1.38608024219576,-12.6600447395717));
#14446=CARTESIAN_POINT('Ctrl Pts',(15.8,2.18750628916194,-14.3692070294775));
#14447=CARTESIAN_POINT('Ctrl Pts',(10.0502525316942,-0.205863042617262,
-9.15961421508102));
#14448=CARTESIAN_POINT('Ctrl Pts',(11.9668350211294,0.590019092973715,-10.8521631299943));
#14449=CARTESIAN_POINT('Ctrl Pts',(13.8834175105647,1.38590122856469,-12.5447120449076));
#14450=CARTESIAN_POINT('Ctrl Pts',(15.8,2.18178336415567,-14.2372609598209));
#14451=CARTESIAN_POINT('Ctrl Pts',(15.8,2.18414382321291,-14.2806055031745));
#14452=CARTESIAN_POINT('Ctrl Pts',(15.8,2.18357641541193,-14.2719548913156));
#14453=CARTESIAN_POINT('Ctrl Pts',(15.8,2.18305667683517,-14.2632951291918));
#14454=CARTESIAN_POINT('Ctrl Pts',(15.8,2.18258459351507,-14.2546262189952));
#14455=CARTESIAN_POINT('Ctrl Pts',(15.8,2.18216015604921,-14.2459481624974));
#14456=CARTESIAN_POINT('Ctrl Pts',(15.8,2.18178336415567,-14.2372609598209));
#14457=CARTESIAN_POINT('Origin',(15.8,3.61104784250494,-14.6201775482978));
#14458=CARTESIAN_POINT('Ctrl Pts',(10.0502525316942,-2.32206279789789,-10.5073910450885));
#14459=CARTESIAN_POINT('Ctrl Pts',(11.1454425256572,-2.01816863800157,-11.7253388222013));
#14460=CARTESIAN_POINT('Ctrl Pts',(12.3775312688656,-1.67628770811821,-13.0955300714531));
#14461=CARTESIAN_POINT('Ctrl Pts',(13.7465187613193,-1.29642000824781,-14.617964792844));
#14462=CARTESIAN_POINT('Ctrl Pts',(14.2941137583009,-1.14447292829965,-15.2269386814004));
#14463=CARTESIAN_POINT('Ctrl Pts',(14.8417087552824,-0.992525848351484,
-15.8359125699568));
#14464=CARTESIAN_POINT('Ctrl Pts',(15.3208543776412,-0.859572153396842,
-16.3687647224436));
#14465=CARTESIAN_POINT('Ctrl Pts',(15.5946518761319,-0.783598613422762,
-16.6732516667218));
#14466=CARTESIAN_POINT('Ctrl Pts',(15.7315506253773,-0.745611843435722,
-16.8254951388609));
#14467=CARTESIAN_POINT('Ctrl Pts',(15.8,-0.726618458442201,-16.9016168749304));
#14468=CARTESIAN_POINT('Ctrl Pts',(10.0502525316942,-2.57345271232946,-10.3973886408451));
#14469=CARTESIAN_POINT('Ctrl Pts',(11.1454425256572,-2.29815463811993,-11.618687280661));
#14470=CARTESIAN_POINT('Ctrl Pts',(12.3775312688656,-1.98887116228557,-12.9928273987101));
#14471=CARTESIAN_POINT('Ctrl Pts',(13.7465187613193,-1.64478997784958,-14.519468077176));
#14472=CARTESIAN_POINT('Ctrl Pts',(14.2941137583009,-1.50716238874916,-15.1301263986154));
#14473=CARTESIAN_POINT('Ctrl Pts',(14.8417087552824,-1.36958497392712,-15.740805777741));
#14474=CARTESIAN_POINT('Ctrl Pts',(15.3208543776412,-1.24918922664557,-16.2751437253593));
#14475=CARTESIAN_POINT('Ctrl Pts',(15.5946518761319,-1.18037249165619,-16.5804716520035));
#14476=CARTESIAN_POINT('Ctrl Pts',(15.7315506253773,-1.14596909077302,-16.7331376997671));
#14477=CARTESIAN_POINT('Ctrl Pts',(15.8,-1.12876296113493,-16.8094688647556));
#14478=CARTESIAN_POINT('Ctrl Pts',(10.0502525316942,-2.93870070814822,-10.189368118401));
#14479=CARTESIAN_POINT('Ctrl Pts',(11.1454425256572,-2.70946206711307,-11.4106316171747));
#14480=CARTESIAN_POINT('Ctrl Pts',(12.3775312688656,-2.45105312324518,-12.7843360022416));
#14481=CARTESIAN_POINT('Ctrl Pts',(13.7465187613194,-2.16445481731473,-14.310894320163));
#14482=CARTESIAN_POINT('Ctrl Pts',(14.2941137583009,-2.04980959621707,-14.9215151635443));
#14483=CARTESIAN_POINT('Ctrl Pts',(14.8417087552824,-1.93510378473095,-15.5321104940175));
#14484=CARTESIAN_POINT('Ctrl Pts',(15.3208543776412,-1.83475492870442,-16.0663892944466));
#14485=CARTESIAN_POINT('Ctrl Pts',(15.5946518761319,-1.77743586902583,-16.3717012113088));
#14486=CARTESIAN_POINT('Ctrl Pts',(15.7315506253773,-1.7487703415134,-16.5243546442885));
#14487=CARTESIAN_POINT('Ctrl Pts',(15.8,-1.7344429264487,-16.6006836129618));
#14488=CARTESIAN_POINT('Ctrl Pts',(10.0502525316942,-3.05808383535427,-9.95881139224219));
#14489=CARTESIAN_POINT('Ctrl Pts',(11.1454425256572,-2.85649631904975,-11.1626816238278));
#14490=CARTESIAN_POINT('Ctrl Pts',(12.3775312688656,-2.62997738853438,-12.5171248305866));
#14491=CARTESIAN_POINT('Ctrl Pts',(13.7465187613193,-2.37801889657081,-14.0219712727573));
#14492=CARTESIAN_POINT('Ctrl Pts',(14.2941137583008,-2.27723855544496,-14.6239108703276));
#14493=CARTESIAN_POINT('Ctrl Pts',(14.8417087552823,-2.17648960137064,-15.225860952321));
#14494=CARTESIAN_POINT('Ctrl Pts',(15.3208543776412,-2.08832456454097,-15.7525640332375));
#14495=CARTESIAN_POINT('Ctrl Pts',(15.5946518761319,-2.03793255455516,-16.0535332175881));
#14496=CARTESIAN_POINT('Ctrl Pts',(15.7315506253773,-2.01273965647872,-16.2040188475872));
#14497=CARTESIAN_POINT('Ctrl Pts',(15.8,-2.00014043670969,-16.2792607370613));
#14498=CARTESIAN_POINT('Ctrl Pts',(10.0502525316942,-3.07559947603194,-9.78147886731912));
#14499=CARTESIAN_POINT('Ctrl Pts',(11.1454425256572,-2.88676320881927,-10.9672359168267));
#14500=CARTESIAN_POINT('Ctrl Pts',(12.3775312688656,-2.67450622091512,-12.3013551830101));
#14501=CARTESIAN_POINT('Ctrl Pts',(13.7465187613194,-2.4384787180816,-13.7835653267336));
#14502=CARTESIAN_POINT('Ctrl Pts',(14.2941137583009,-2.34406982037813,-14.3764510158762));
#14503=CARTESIAN_POINT('Ctrl Pts',(14.8417087552824,-2.2496825286364,-14.9693534649946));
#14504=CARTESIAN_POINT('Ctrl Pts',(15.3208543776412,-2.16708696976893,-15.4881379273167));
#14505=CARTESIAN_POINT('Ctrl Pts',(15.5946518761319,-2.11988125471031,-15.7845797896778));
#14506=CARTESIAN_POINT('Ctrl Pts',(15.7315506253773,-2.09628053589475,-15.9328023798814));
#14507=CARTESIAN_POINT('Ctrl Pts',(15.8,-2.08447826919396,-16.0069121954757));
#14508=CARTESIAN_POINT('Ctrl Pts',(10.0502525316942,-3.10223684531881,-9.60383008034201));
#14509=CARTESIAN_POINT('Ctrl Pts',(11.1454425256572,-2.92542368552958,-10.7718807970721));
#14510=CARTESIAN_POINT('Ctrl Pts',(12.3775312688656,-2.72674232124834,-12.0859609655105));
#14511=CARTESIAN_POINT('Ctrl Pts',(13.7465187613193,-2.50574851695231,-13.5460266034681));
#14512=CARTESIAN_POINT('Ctrl Pts',(14.2941137583008,-2.41735366657092,-14.1300531231308));
#14513=CARTESIAN_POINT('Ctrl Pts',(14.8417087552824,-2.32898625556579,-14.7140823594691));
#14514=CARTESIAN_POINT('Ctrl Pts',(15.3208543776412,-2.25165628918294,-15.2251071015168));
#14515=CARTESIAN_POINT('Ctrl Pts',(15.5946518761319,-2.20745725592095,-15.5171202021386));
#14516=CARTESIAN_POINT('Ctrl Pts',(15.7315506253773,-2.18536045543708,-15.6631270213657));
#14517=CARTESIAN_POINT('Ctrl Pts',(15.8,-2.17430963295026,-15.7361301911613));
#14518=CARTESIAN_POINT('Ctrl Pts',(10.0502525316942,-3.16416975479849,-9.33616641898042));
#14519=CARTESIAN_POINT('Ctrl Pts',(11.1454425256572,-3.00789330574877,-10.4789053528453));
#14520=CARTESIAN_POINT('Ctrl Pts',(12.3775312688656,-2.83212323706007,-11.7645911992084));
#14521=CARTESIAN_POINT('Ctrl Pts',(13.7465187613193,-2.6367816468882,-13.1930250082462));
#14522=CARTESIAN_POINT('Ctrl Pts',(14.2941137583008,-2.55864547926934,-13.7643997282132));
#14523=CARTESIAN_POINT('Ctrl Pts',(14.8417087552823,-2.48051412346291,-14.3357867368398));
#14524=CARTESIAN_POINT('Ctrl Pts',(15.3208543776412,-2.4121476997586,-14.8357465708549));
#14525=CARTESIAN_POINT('Ctrl Pts',(15.5946518761319,-2.37307933395524,-15.1214332106675));
#14526=CARTESIAN_POINT('Ctrl Pts',(15.7315506253773,-2.35354562736142,-15.2642777469938));
#14527=CARTESIAN_POINT('Ctrl Pts',(15.8,-2.34377834929582,-15.3356989303604));
#14528=CARTESIAN_POINT('Ctrl Pts',(10.0502525316942,-3.14987939962279,-9.08015411140624));
#14529=CARTESIAN_POINT('Ctrl Pts',(11.1454425256572,-3.0067293155267,-10.19428901683));
#14530=CARTESIAN_POINT('Ctrl Pts',(12.3775312688656,-2.84574388114627,-11.4477380681646));
#14531=CARTESIAN_POINT('Ctrl Pts',(13.7465187613193,-2.66681194224705,-12.8404112867165));
#14532=CARTESIAN_POINT('Ctrl Pts',(14.2941137583008,-2.59523983509501,-13.3974811152093));
#14533=CARTESIAN_POINT('Ctrl Pts',(14.8417087552823,-2.52367459367681,-13.9545565014729));
#14534=CARTESIAN_POINT('Ctrl Pts',(15.3208543776412,-2.46105288517697,-14.4419957464975));
#14535=CARTESIAN_POINT('Ctrl Pts',(15.5946518761319,-2.42526642923796,-14.7205303350335));
#14536=CARTESIAN_POINT('Ctrl Pts',(15.7315506253773,-2.40737388088825,-14.8597981794497));
#14537=CARTESIAN_POINT('Ctrl Pts',(15.8,-2.39842700063224,-14.9294316110386));
#14538=CARTESIAN_POINT('Ctrl Pts',(10.0502525316942,-3.10442465522081,-8.83780343943476));
#14539=CARTESIAN_POINT('Ctrl Pts',(11.1454425256572,-2.96904269314958,-9.92307916160989));
#14540=CARTESIAN_POINT('Ctrl Pts',(12.3775312688656,-2.81681208487056,-11.1440266947135));
#14541=CARTESIAN_POINT('Ctrl Pts',(13.7465187613194,-2.64759182043347,-12.5006225450517));
#14542=CARTESIAN_POINT('Ctrl Pts',(14.2941137583009,-2.5799045625987,-13.0432610264625));
#14543=CARTESIAN_POINT('Ctrl Pts',(14.8417087552824,-2.51222601461465,-13.585900959023));
#14544=CARTESIAN_POINT('Ctrl Pts',(15.3208543776412,-2.45300459283688,-14.0607104514503));
#14545=CARTESIAN_POINT('Ctrl Pts',(15.594651876132,-2.41916045348293,-14.3320296071118));
#14546=CARTESIAN_POINT('Ctrl Pts',(15.7315506253773,-2.40223924596973,-14.4676893285877));
#14547=CARTESIAN_POINT('Ctrl Pts',(15.8,-2.39377787334028,-14.5355190612237));
#14548=CARTESIAN_POINT('Ctrl Pts',(10.0502525316942,-3.06201554081689,-8.72224646189196));
#14549=CARTESIAN_POINT('Ctrl Pts',(11.1454425256572,-2.92828468444751,-9.79262845293104));
#14550=CARTESIAN_POINT('Ctrl Pts',(12.3775312688656,-2.77780914227504,-10.9969124481398));
#14551=CARTESIAN_POINT('Ctrl Pts',(13.7465187613193,-2.61064282371592,-12.3349000504671));
#14552=CARTESIAN_POINT('Ctrl Pts',(14.2941137583009,-2.54377597211689,-12.870096284426));
#14553=CARTESIAN_POINT('Ctrl Pts',(14.8417087552824,-2.47690579066087,-13.4053047729009));
#14554=CARTESIAN_POINT('Ctrl Pts',(15.3208543776412,-2.41839541117503,-13.8736084123374));
#14555=CARTESIAN_POINT('Ctrl Pts',(15.5946518761319,-2.38496218052017,-14.1412058111469));
#14556=CARTESIAN_POINT('Ctrl Pts',(15.7315506253773,-2.3682452355795,-14.2750057235919));
#14557=CARTESIAN_POINT('Ctrl Pts',(15.8,-2.35988705705642,-14.3419045980318));
#14558=CARTESIAN_POINT('Ctrl Pts',(10.0502525316942,-3.02626384252387,-8.64769560732005));
#14559=CARTESIAN_POINT('Ctrl Pts',(11.1454425256572,-2.89260526381667,-9.70806748165927));
#14560=CARTESIAN_POINT('Ctrl Pts',(12.3775312688656,-2.74223936277106,-10.9009858402909));
#14561=CARTESIAN_POINT('Ctrl Pts',(13.7465187613193,-2.57516613938705,-12.2264506832149));
#14562=CARTESIAN_POINT('Ctrl Pts',(14.2941137583009,-2.50833685003344,-12.7566366203845));
#14563=CARTESIAN_POINT('Ctrl Pts',(14.8417087552824,-2.44150756067984,-13.2868225575541));
#14564=CARTESIAN_POINT('Ctrl Pts',(15.3208543776412,-2.38303193249543,-13.7507352525775));
#14565=CARTESIAN_POINT('Ctrl Pts',(15.5946518761319,-2.34961728781863,-14.0158282211623));
#14566=CARTESIAN_POINT('Ctrl Pts',(15.7315506253773,-2.33290996548023,-14.1483747054547));
#14567=CARTESIAN_POINT('Ctrl Pts',(15.8,-2.32455630431103,-14.2146479476009));
#14568=CARTESIAN_POINT('Ctrl Pts',(15.8,-2.33570557485288,-14.2566004799664));
#14569=CARTESIAN_POINT('Ctrl Pts',(15.8,-2.33357202566325,-14.2481979205348));
#14570=CARTESIAN_POINT('Ctrl Pts',(15.8,-2.33139031275994,-14.2398013892846));
#14571=CARTESIAN_POINT('Ctrl Pts',(15.8,-2.32916045010432,-14.2314108839843));
#14572=CARTESIAN_POINT('Ctrl Pts',(15.8,-2.326882447186,-14.2230264034132));
#14573=CARTESIAN_POINT('Ctrl Pts',(15.8,-2.32455630431103,-14.2146479476009));
#14574=CARTESIAN_POINT('Origin',(15.8,-1.08357274193521,-15.0204902775358));
#14575=CARTESIAN_POINT('Ctrl Pts',(10.0502525316942,-5.45537535466284,-9.2755658561365));
#14576=CARTESIAN_POINT('Ctrl Pts',(11.1454425256572,-5.54272139501843,-10.527811485966));
#14577=CARTESIAN_POINT('Ctrl Pts',(12.3775312688656,-5.64098569041847,-11.9365878195243));
#14578=CARTESIAN_POINT('Ctrl Pts',(13.7465187613193,-5.75016824086296,-13.5018948568112));
#14579=CARTESIAN_POINT('Ctrl Pts',(14.2941137583009,-5.79384126104075,-14.1280176717259));
#14580=CARTESIAN_POINT('Ctrl Pts',(14.8417087552824,-5.83751428121855,-14.7541404866407));
#14581=CARTESIAN_POINT('Ctrl Pts',(15.3208543776412,-5.87572817387412,-15.3019979496911));
#14582=CARTESIAN_POINT('Ctrl Pts',(15.5946518761319,-5.89756468396302,-15.6150593571485));
#14583=CARTESIAN_POINT('Ctrl Pts',(15.7315506253773,-5.90848293900746,-15.7715900608772));
#14584=CARTESIAN_POINT('Ctrl Pts',(15.8,-5.91394206652969,-15.8498554127416));
#14585=CARTESIAN_POINT('Ctrl Pts',(10.0502525316942,-5.66046875858054,-9.09326359699885));
#14586=CARTESIAN_POINT('Ctrl Pts',(11.1454425256572,-5.77604676609019,-10.3398594101876));
#14587=CARTESIAN_POINT('Ctrl Pts',(12.3775312688656,-5.90654052031257,-11.7423187718539));
#14588=CARTESIAN_POINT('Ctrl Pts',(13.7465187613193,-6.05105541408884,-13.3005670731329));
#14589=CARTESIAN_POINT('Ctrl Pts',(14.2941137583009,-6.10886731837785,-13.9238668895967));
#14590=CARTESIAN_POINT('Ctrl Pts',(14.8417087552824,-6.16673138983645,-14.5471710567224));
#14591=CARTESIAN_POINT('Ctrl Pts',(15.3208543776412,-6.21734620559881,-15.0925608480023));
#14592=CARTESIAN_POINT('Ctrl Pts',(15.5946518761319,-6.24624880770452,-15.4042104768461));
#14593=CARTESIAN_POINT('Ctrl Pts',(15.7315506253773,-6.26070528969669,-15.5600357233504));
#14594=CARTESIAN_POINT('Ctrl Pts',(15.8,-6.26792891516604,-15.6379479616747));
#14595=CARTESIAN_POINT('Ctrl Pts',(10.0502525316942,-5.94355560685309,-8.78255765938311));
#14596=CARTESIAN_POINT('Ctrl Pts',(11.1454425256572,-6.10292787924083,-10.0148869038525));
#14597=CARTESIAN_POINT('Ctrl Pts',(12.3775312688656,-6.2816544949474,-11.4012092316412));
#14598=CARTESIAN_POINT('Ctrl Pts',(13.7465187613194,-6.48081852219944,-12.9416164381759));
#14599=CARTESIAN_POINT('Ctrl Pts',(14.2941137583009,-6.56047693355264,-13.5577787105922));
#14600=CARTESIAN_POINT('Ctrl Pts',(14.8417087552824,-6.64007218801815,-14.1739356301478));
#14601=CARTESIAN_POINT('Ctrl Pts',(15.3208543776412,-6.70973770503938,-14.7130746018355));
#14602=CARTESIAN_POINT('Ctrl Pts',(15.594651876132,-6.74957096648566,-15.0211560817903));
#14603=CARTESIAN_POINT('Ctrl Pts',(15.7315506253773,-6.76948132483471,-15.1751962901528));
#14604=CARTESIAN_POINT('Ctrl Pts',(15.8,-6.77944209185894,-15.2522168679322));
#14605=CARTESIAN_POINT('Ctrl Pts',(10.0502525316942,-5.98584659003549,-8.52639512605652));
#14606=CARTESIAN_POINT('Ctrl Pts',(11.1454425256572,-6.16614182963237,-9.73363772297167));
#14607=CARTESIAN_POINT('Ctrl Pts',(12.3775312688656,-6.36925721416675,-11.0917875706281));
#14608=CARTESIAN_POINT('Ctrl Pts',(13.7465187613193,-6.59465188812854,-12.6008409910269));
#14609=CARTESIAN_POINT('Ctrl Pts',(14.2941137583008,-6.68481335297615,-13.2044623836355));
#14610=CARTESIAN_POINT('Ctrl Pts',(14.8417087552823,-6.77500635669625,-13.8080839907189));
#14611=CARTESIAN_POINT('Ctrl Pts',(15.3208543776412,-6.85391541259334,-14.3362528301216));
#14612=CARTESIAN_POINT('Ctrl Pts',(15.5946518761319,-6.89899411967348,-14.6380635126529));
#14613=CARTESIAN_POINT('Ctrl Pts',(15.7315506253773,-6.92153660547059,-14.7889688752189));
#14614=CARTESIAN_POINT('Ctrl Pts',(15.8,-6.9328050579454,-14.8644215375261));
#14615=CARTESIAN_POINT('Ctrl Pts',(10.0502525316942,-5.94770436886828,-8.35233000922534));
#14616=CARTESIAN_POINT('Ctrl Pts',(11.1454425256572,-6.13452948592056,-9.5384055936255));
#14617=CARTESIAN_POINT('Ctrl Pts',(12.3775312688656,-6.34492663085593,-10.8728200811769));
#14618=CARTESIAN_POINT('Ctrl Pts',(13.7465187613193,-6.57847782979355,-12.3554217499083));
#14619=CARTESIAN_POINT('Ctrl Pts',(14.2941137583008,-6.67190108779269,-12.9484634259519));
#14620=CARTESIAN_POINT('Ctrl Pts',(14.8417087552824,-6.76534871907581,-13.541513949349));
#14621=CARTESIAN_POINT('Ctrl Pts',(15.3208543776412,-6.84710780571679,-14.0604304019321));
#14622=CARTESIAN_POINT('Ctrl Pts',(15.5946518761319,-6.89381786952799,-14.3569506718));
#14623=CARTESIAN_POINT('Ctrl Pts',(15.7315506253773,-6.91717532204614,-14.5052116854016));
#14624=CARTESIAN_POINT('Ctrl Pts',(15.8,-6.92885189186191,-14.5793414094266));
#14625=CARTESIAN_POINT('Ctrl Pts',(10.0502525316942,-5.91814205125966,-8.1751443698686));
#14626=CARTESIAN_POINT('Ctrl Pts',(11.1454425256572,-6.11093026523681,-9.34066488658195));
#14627=CARTESIAN_POINT('Ctrl Pts',(12.3775312688656,-6.32804641946555,-10.6518240329443));
#14628=CARTESIAN_POINT('Ctrl Pts',(13.7465187613193,-6.56905244176938,-12.1087200255634));
#14629=CARTESIAN_POINT('Ctrl Pts',(14.2941137583008,-6.66545776271567,-12.6914777697296));
#14630=CARTESIAN_POINT('Ctrl Pts',(14.8417087552823,-6.76188862893655,-13.2742297865971));
#14631=CARTESIAN_POINT('Ctrl Pts',(15.3208543776412,-6.84625768114735,-13.7841395850464));
#14632=CARTESIAN_POINT('Ctrl Pts',(15.5946518761319,-6.89445870116997,-14.0755188249216));
#14633=CARTESIAN_POINT('Ctrl Pts',(15.7315506253773,-6.9185617481891,-14.2212078760573));
#14634=CARTESIAN_POINT('Ctrl Pts',(15.8,-6.93061101156267,-14.2940529083518));
#14635=CARTESIAN_POINT('Ctrl Pts',(10.0502525316942,-5.8943312499999,-7.90144264462466));
#14636=CARTESIAN_POINT('Ctrl Pts',(11.1454425256572,-6.09882926548584,-9.03654403267794));
#14637=CARTESIAN_POINT('Ctrl Pts',(12.3775312688656,-6.32895925304843,-10.3136205759385));
#14638=CARTESIAN_POINT('Ctrl Pts',(13.7465187613193,-6.58458807992399,-11.7325052253954));
#14639=CARTESIAN_POINT('Ctrl Pts',(14.2941137583008,-6.68684049565601,-12.3000601956136));
#14640=CARTESIAN_POINT('Ctrl Pts',(14.8417087552823,-6.7891006747503,-12.86762490695));
#14641=CARTESIAN_POINT('Ctrl Pts',(15.3208543776411,-6.87857591366296,-13.364240995629));
#14642=CARTESIAN_POINT('Ctrl Pts',(15.5946518761319,-6.92970162298621,-13.6480178551891));
#14643=CARTESIAN_POINT('Ctrl Pts',(15.7315506253773,-6.95526524865974,-13.7899072524002));
#14644=CARTESIAN_POINT('Ctrl Pts',(15.8,-6.96804637462761,-13.8608510891535));
#14645=CARTESIAN_POINT('Ctrl Pts',(10.0502525316942,-5.80163007173558,-7.66237562613099));
#14646=CARTESIAN_POINT('Ctrl Pts',(11.1454425256572,-6.00977287125004,-8.76621669669801));
#14647=CARTESIAN_POINT('Ctrl Pts',(12.3775312688656,-6.24400287259235,-10.008064757174));
#14648=CARTESIAN_POINT('Ctrl Pts',(13.7465187613193,-6.50418764618811,-11.3878685250288));
#14649=CARTESIAN_POINT('Ctrl Pts',(14.2941137583008,-6.60826243593386,-11.9397903730643));
#14650=CARTESIAN_POINT('Ctrl Pts',(14.8417087552823,-6.71234494803684,-12.4917152115347));
#14651=CARTESIAN_POINT('Ctrl Pts',(15.3208543776411,-6.80341474110257,-12.9746485138656));
#14652=CARTESIAN_POINT('Ctrl Pts',(15.5946518761319,-6.85545164006593,-13.2506092458454));
#14653=CARTESIAN_POINT('Ctrl Pts',(15.7315506253773,-6.88147085648712,-13.388589908828));
#14654=CARTESIAN_POINT('Ctrl Pts',(15.8,-6.89447978145678,-13.4575799757384));
#14655=CARTESIAN_POINT('Ctrl Pts',(10.0502525316942,-5.68351040711504,-7.44593237535689));
#14656=CARTESIAN_POINT('Ctrl Pts',(11.1454425256572,-5.89012315163304,-8.51992624992032));
#14657=CARTESIAN_POINT('Ctrl Pts',(12.3775312688656,-6.12263633930509,-9.72815762348205));
#14658=CARTESIAN_POINT('Ctrl Pts',(13.7465187613194,-6.38090895110341,-11.0706489050023));
#14659=CARTESIAN_POINT('Ctrl Pts',(14.2941137583009,-6.4842189332274,-11.60764526865));
#14660=CARTESIAN_POINT('Ctrl Pts',(14.8417087552824,-6.58753713858487,-12.1446403255654));
#14661=CARTESIAN_POINT('Ctrl Pts',(15.3208543776412,-6.6779380072571,-12.6145114073305));
#14662=CARTESIAN_POINT('Ctrl Pts',(15.594651876132,-6.72959247024461,-12.8830096730692));
#14663=CARTESIAN_POINT('Ctrl Pts',(15.7315506253773,-6.755420518422,-13.0172586761616));
#14664=CARTESIAN_POINT('Ctrl Pts',(15.8,-6.76833381495438,-13.0843832933218));
#14665=CARTESIAN_POINT('Ctrl Pts',(10.0502525316942,-5.60747221894231,-7.34913449516209));
#14666=CARTESIAN_POINT('Ctrl Pts',(11.1454425256572,-5.81105284226644,-8.40845336995523));
#14667=CARTESIAN_POINT('Ctrl Pts',(12.3775312688656,-6.04008639989118,-9.60029668798142));
#14668=CARTESIAN_POINT('Ctrl Pts',(13.7465187613193,-6.29456266363366,-10.9244551954278));
#14669=CARTESIAN_POINT('Ctrl Pts',(14.2941137583009,-6.3963532371211,-11.4541199893924));
#14670=CARTESIAN_POINT('Ctrl Pts',(14.8417087552824,-6.49814440704391,-11.9837969855611));
#14671=CARTESIAN_POINT('Ctrl Pts',(15.3208543776412,-6.58721149497458,-12.4472605569962));
#14672=CARTESIAN_POINT('Ctrl Pts',(15.5946518761319,-6.63810674341679,-12.7120921703849));
#14673=CARTESIAN_POINT('Ctrl Pts',(15.7315506253773,-6.66355442687238,-12.8445091889311));
#14674=CARTESIAN_POINT('Ctrl Pts',(15.8,-6.67627821583014,-12.9107166186057));
#14675=CARTESIAN_POINT('Ctrl Pts',(10.0502525316942,-5.55043285230422,-7.28928030147641));
#14676=CARTESIAN_POINT('Ctrl Pts',(11.1454425256572,-5.75098891959401,-8.33905665452735));
#14677=CARTESIAN_POINT('Ctrl Pts',(12.3775312688656,-5.97661449529503,-9.52005505170966));
#14678=CARTESIAN_POINT('Ctrl Pts',(13.7465187613193,-6.22730957940728,-10.8322754930233));
#14679=CARTESIAN_POINT('Ctrl Pts',(14.2941137583009,-6.32758761305217,-11.3571636695488));
#14680=CARTESIAN_POINT('Ctrl Pts',(14.8417087552824,-6.42786564669707,-11.8820518460743));
#14681=CARTESIAN_POINT('Ctrl Pts',(15.3208543776412,-6.51560892613635,-12.3413290005341));
#14682=CARTESIAN_POINT('Ctrl Pts',(15.5946518761319,-6.56574794295881,-12.6037730887968));
#14683=CARTESIAN_POINT('Ctrl Pts',(15.7315506253773,-6.59081745137003,-12.7349951329282));
#14684=CARTESIAN_POINT('Ctrl Pts',(15.8,-6.60335220557564,-12.8006061549939));
#14685=CARTESIAN_POINT('Ctrl Pts',(15.8,-6.62691983743441,-12.8370600702028));
#14686=CARTESIAN_POINT('Ctrl Pts',(15.8,-6.62229417791417,-12.8297280642598));
#14687=CARTESIAN_POINT('Ctrl Pts',(15.8,-6.61762457479065,-12.8224166748639));
#14688=CARTESIAN_POINT('Ctrl Pts',(15.8,-6.61291104065239,-12.8151258955788));
#14689=CARTESIAN_POINT('Ctrl Pts',(15.8,-6.60815358414732,-12.8078557223109));
#14690=CARTESIAN_POINT('Ctrl Pts',(15.8,-6.60335220557564,-12.8006061549939));
#14691=CARTESIAN_POINT('Origin',(15.8,-5.67212567669951,-13.950492764499));
#14692=CARTESIAN_POINT('Ctrl Pts',(10.0502525316942,-8.05467776187827,-7.13578365451838));
#14693=CARTESIAN_POINT('Ctrl Pts',(11.1454425256572,-8.52471396348012,-8.29974860990865));
#14694=CARTESIAN_POINT('Ctrl Pts',(12.3775312688656,-9.05350469028219,-9.6092091847227));
#14695=CARTESIAN_POINT('Ctrl Pts',(13.7465187613193,-9.6410499422845,-11.0641653789605));
#14696=CARTESIAN_POINT('Ctrl Pts',(14.2941137583009,-9.87606804308543,-11.6461478566557));
#14697=CARTESIAN_POINT('Ctrl Pts',(14.8417087552824,-10.1110861438864,-12.2281303343508));
#14698=CARTESIAN_POINT('Ctrl Pts',(15.3208543776412,-10.3167269820872,-12.737365002334));
#14699=CARTESIAN_POINT('Ctrl Pts',(15.5946518761319,-10.4342360324876,-13.0283562411816));
#14700=CARTESIAN_POINT('Ctrl Pts',(15.7315506253773,-10.4929905576879,-13.1738518606054));
#14701=CARTESIAN_POINT('Ctrl Pts',(15.8,-10.522367820288,-13.2465996703173));
#14702=CARTESIAN_POINT('Ctrl Pts',(10.0502525316942,-8.19339868393687,-6.89902655578542));
#14703=CARTESIAN_POINT('Ctrl Pts',(11.1454425256572,-8.68853919251131,-8.04889405860839));
#14704=CARTESIAN_POINT('Ctrl Pts',(12.3775312688656,-9.24602752966092,-9.34238794408146));
#14705=CARTESIAN_POINT('Ctrl Pts',(13.7465187613193,-9.86499535005157,-10.779712402918));
#14706=CARTESIAN_POINT('Ctrl Pts',(14.2941137583009,-10.1125880646808,-11.354640872798));
#14707=CARTESIAN_POINT('Ctrl Pts',(14.8417087552824,-10.3602324253388,-11.9295571981554));
#14708=CARTESIAN_POINT('Ctrl Pts',(15.3208543776412,-10.5769051976768,-12.4326127553978));
#14709=CARTESIAN_POINT('Ctrl Pts',(15.5946518761319,-10.7006983402633,-12.7200777462785));
#14710=CARTESIAN_POINT('Ctrl Pts',(15.7315506253773,-10.7626000339661,-12.8638090371883));
#14711=CARTESIAN_POINT('Ctrl Pts',(15.8,-10.793546315752,-12.9356757561148));
#14712=CARTESIAN_POINT('Ctrl Pts',(10.0502525316942,-8.36661813687798,-6.51604789180993));
#14713=CARTESIAN_POINT('Ctrl Pts',(11.1454425256572,-8.8990008542554,-7.63881390938367));
#14714=CARTESIAN_POINT('Ctrl Pts',(12.3775312688656,-9.49738068383039,-8.90205445633838));
#14715=CARTESIAN_POINT('Ctrl Pts',(13.7465187613194,-10.1628080503653,-10.3055239107478));
#14716=CARTESIAN_POINT('Ctrl Pts',(14.2941137583009,-10.4289722391039,-10.8669132727127));
#14717=CARTESIAN_POINT('Ctrl Pts',(14.8417087552824,-10.6950739523901,-11.4283172433782));
#14718=CARTESIAN_POINT('Ctrl Pts',(15.3208543776412,-10.9279323587878,-11.9195411796877));
#14719=CARTESIAN_POINT('Ctrl Pts',(15.594651876132,-11.0610183419671,-12.2002349513456));
#14720=CARTESIAN_POINT('Ctrl Pts',(15.7315506253773,-11.1275551370522,-12.3405832861097));
#14721=CARTESIAN_POINT('Ctrl Pts',(15.8,-11.1608290568883,-12.4107561622081));
#14722=CARTESIAN_POINT('Ctrl Pts',(10.0502525316942,-8.32768215464935,-6.25935291859366));
#14723=CARTESIAN_POINT('Ctrl Pts',(11.1454425256572,-8.87221159590509,-7.35179456409856));
#14724=CARTESIAN_POINT('Ctrl Pts',(12.3775312688656,-9.48507728715609,-8.58070593097969));
#14725=CARTESIAN_POINT('Ctrl Pts',(13.7465187613193,-10.1657641132886,-9.94625006691877));
#14726=CARTESIAN_POINT('Ctrl Pts',(14.2941137583008,-10.4380421577189,-10.4924666723322));
#14727=CARTESIAN_POINT('Ctrl Pts',(14.8417087552823,-10.7103508393265,-11.0386735802612));
#14728=CARTESIAN_POINT('Ctrl Pts',(15.3208543776412,-10.9486114186505,-11.5166076371098));
#14729=CARTESIAN_POINT('Ctrl Pts',(15.5946518761319,-11.0847485338421,-11.7897165434404));
#14730=CARTESIAN_POINT('Ctrl Pts',(15.7315506253773,-11.1528201301259,-11.9262700347798));
#14731=CARTESIAN_POINT('Ctrl Pts',(15.8,-11.1868532202043,-11.9945476376238));
#14732=CARTESIAN_POINT('Ctrl Pts',(10.0502525316942,-8.23761851725689,-6.10559301495173));
#14733=CARTESIAN_POINT('Ctrl Pts',(11.1454425256572,-8.78181727442991,-7.17588579216885));
#14734=CARTESIAN_POINT('Ctrl Pts',(12.3775312688656,-9.39427431712614,-8.37997276877534));
#14735=CARTESIAN_POINT('Ctrl Pts',(13.7465187613193,-10.0745443941304,-9.71783944471699));
#14736=CARTESIAN_POINT('Ctrl Pts',(14.2941137583009,-10.3466552894421,-10.2529862083793));
#14737=CARTESIAN_POINT('Ctrl Pts',(14.8417087552824,-10.61879266668,-10.7881338344522));
#14738=CARTESIAN_POINT('Ctrl Pts',(15.3208543776412,-10.856904645461,-11.2563877393682));
#14739=CARTESIAN_POINT('Ctrl Pts',(15.5946518761319,-10.9929584447386,-11.5239610675182));
#14740=CARTESIAN_POINT('Ctrl Pts',(15.7315506253773,-11.060987970935,-11.6577478171298));
#14741=CARTESIAN_POINT('Ctrl Pts',(15.8,-11.0950003932583,-11.7246411157058));
#14742=CARTESIAN_POINT('Ctrl Pts',(10.0502525316942,-8.15474945546092,-5.94621492062453));
#14743=CARTESIAN_POINT('Ctrl Pts',(11.1454425256572,-8.69826758958589,-6.99511596848632));
#14744=CARTESIAN_POINT('Ctrl Pts',(12.3775312688656,-9.30992859260386,-8.17501015002259));
#14745=CARTESIAN_POINT('Ctrl Pts',(13.7465187613193,-9.98934507962172,-9.48612538727718));
#14746=CARTESIAN_POINT('Ctrl Pts',(14.2941137583008,-10.2611141666576,-10.0105700158496));
#14747=CARTESIAN_POINT('Ctrl Pts',(14.8417087552823,-10.532906293941,-10.535001088446));
#14748=CARTESIAN_POINT('Ctrl Pts',(15.3208543776412,-10.7707172481292,-10.9938824879741));
#14749=CARTESIAN_POINT('Ctrl Pts',(15.5946518761319,-10.9066003574976,-11.2561056460575));
#14750=CARTESIAN_POINT('Ctrl Pts',(15.7315506253773,-10.9745441973833,-11.3872158805765));
#14751=CARTESIAN_POINT('Ctrl Pts',(15.8,-11.0085140807661,-11.4527721960679));
#14752=CARTESIAN_POINT('Ctrl Pts',(10.0502525316942,-8.04752551167497,-5.69326714724858));
#14753=CARTESIAN_POINT('Ctrl Pts',(11.1454425256572,-8.59278030111935,-6.70961935691122));
#14754=CARTESIAN_POINT('Ctrl Pts',(12.3775312688656,-9.20628631668585,-7.85307681747465));
#14755=CARTESIAN_POINT('Ctrl Pts',(13.7465187613193,-9.8878635484672,-9.12352275260843));
#14756=CARTESIAN_POINT('Ctrl Pts',(14.2941137583008,-10.1604955992679,-9.63170187793887));
#14757=CARTESIAN_POINT('Ctrl Pts',(14.8417087552824,-10.4331383564046,-10.1398879487016));
#14758=CARTESIAN_POINT('Ctrl Pts',(15.3208543776412,-10.6716974431005,-10.5845486031013));
#14759=CARTESIAN_POINT('Ctrl Pts',(15.5946518761319,-10.8080128020807,-10.8386377334453));
#14760=CARTESIAN_POINT('Ctrl Pts',(15.7315506253773,-10.8761715434576,-10.9656829874862));
#14761=CARTESIAN_POINT('Ctrl Pts',(15.8,-10.9102499677978,-11.0292050005901));
#14762=CARTESIAN_POINT('Ctrl Pts',(10.0502525316942,-7.88548479029562,-5.49454791241254));
#14763=CARTESIAN_POINT('Ctrl Pts',(11.1454425256572,-8.42454600598801,-6.48004349322278));
#14764=CARTESIAN_POINT('Ctrl Pts',(12.3775312688656,-9.03106484753224,-7.58873003819356));
#14765=CARTESIAN_POINT('Ctrl Pts',(13.7465187613193,-9.70489831419834,-8.82059988637913));
#14766=CARTESIAN_POINT('Ctrl Pts',(14.2941137583008,-9.97443262085556,-9.31334787493982));
#14767=CARTESIAN_POINT('Ctrl Pts',(14.8417087552823,-10.2439754326772,-9.80609631914575));
#14768=CARTESIAN_POINT('Ctrl Pts',(15.3208543776411,-10.4798227509908,-10.237251066285));
#14769=CARTESIAN_POINT('Ctrl Pts',(15.5946518761319,-10.614589374912,-10.4836250322036));
#14770=CARTESIAN_POINT('Ctrl Pts',(15.7315506253773,-10.6819735304405,-10.6068120603551));
#14771=CARTESIAN_POINT('Ctrl Pts',(15.8,-10.7156648564213,-10.6684055341557));
#14772=CARTESIAN_POINT('Ctrl Pts',(10.0502525316942,-7.70626127860213,-5.32519947010611));
#14773=CARTESIAN_POINT('Ctrl Pts',(11.1454425256572,-8.23464403472029,-6.28278149366022));
#14774=CARTESIAN_POINT('Ctrl Pts',(12.3775312688656,-8.82914182271552,-7.36002740501521));
#14775=CARTESIAN_POINT('Ctrl Pts',(13.7465187613194,-9.48962649341726,-8.55700179652725));
#14776=CARTESIAN_POINT('Ctrl Pts',(14.2941137583009,-9.7538211861417,-9.03579113757913));
#14777=CARTESIAN_POINT('Ctrl Pts',(14.8417087552824,-10.0180235007137,-9.5145766369121));
#14778=CARTESIAN_POINT('Ctrl Pts',(15.3208543776412,-10.2491981583259,-9.93351514221373));
#14779=CARTESIAN_POINT('Ctrl Pts',(15.594651876132,-10.3812950302632,-10.172910051869));
#14780=CARTESIAN_POINT('Ctrl Pts',(15.7315506253773,-10.4473442221897,-10.2926071256634));
#14781=CARTESIAN_POINT('Ctrl Pts',(15.8,-10.4803681444471,-10.3524560021355));
#14782=CARTESIAN_POINT('Ctrl Pts',(10.0502525316942,-7.60403044672135,-5.25663803961482));
#14783=CARTESIAN_POINT('Ctrl Pts',(11.1454425256572,-8.12499465989843,-6.20120028598869));
#14784=CARTESIAN_POINT('Ctrl Pts',(12.3775312688656,-8.71111815506916,-7.26393484617381));
#14785=CARTESIAN_POINT('Ctrl Pts',(13.7465187613193,-9.36232701259537,-8.44464710847935));
#14786=CARTESIAN_POINT('Ctrl Pts',(14.2941137583009,-9.62281103116557,-8.91693326542987));
#14787=CARTESIAN_POINT('Ctrl Pts',(14.8417087552824,-9.88329944620756,-9.38923099717744));
#14788=CARTESIAN_POINT('Ctrl Pts',(15.3208543776412,-10.1112254436565,-9.80248791688055));
#14789=CARTESIAN_POINT('Ctrl Pts',(15.5946518761319,-10.2414671792814,-10.0386302748779));
#14790=CARTESIAN_POINT('Ctrl Pts',(15.7315506253773,-10.3065884831493,-10.1567026019));
#14791=CARTESIAN_POINT('Ctrl Pts',(15.8,-10.3391487464728,-10.2157377422983));
#14792=CARTESIAN_POINT('Ctrl Pts',(10.0502525316942,-7.53128682236137,-5.21733945232202));
#14793=CARTESIAN_POINT('Ctrl Pts',(11.1454425256572,-8.04642571042556,-6.15376086042613));
#14794=CARTESIAN_POINT('Ctrl Pts',(12.3775312688656,-8.62595695949777,-7.20723494454326));
#14795=CARTESIAN_POINT('Ctrl Pts',(13.7465187613193,-9.269880569578,-8.3777617046734));
#14796=CARTESIAN_POINT('Ctrl Pts',(14.2941137583009,-9.52745001361009,-8.84597240872545));
#14797=CARTESIAN_POINT('Ctrl Pts',(14.8417087552824,-9.78501945764219,-9.31418311277751));
#14798=CARTESIAN_POINT('Ctrl Pts',(15.3208543776412,-10.0103927211703,-9.72386747882306));
#14799=CARTESIAN_POINT('Ctrl Pts',(15.5946518761319,-10.1391774431863,-9.95797283084909));
#14800=CARTESIAN_POINT('Ctrl Pts',(15.7315506253773,-10.2035698041943,-10.0750255068621));
#14801=CARTESIAN_POINT('Ctrl Pts',(15.8,-10.2357659846983,-10.1335518448686));
#14802=CARTESIAN_POINT('Ctrl Pts',(15.8,-10.2694450138623,-10.160938779711));
#14803=CARTESIAN_POINT('Ctrl Pts',(15.8,-10.2627800357942,-10.1553950350833));
#14804=CARTESIAN_POINT('Ctrl Pts',(15.8,-10.2560796357392,-10.1498844772774));
#14805=CARTESIAN_POINT('Ctrl Pts',(15.8,-10.2493438236809,-10.1444070962816));
#14806=CARTESIAN_POINT('Ctrl Pts',(15.8,-10.242572606579,-10.1389628855307));
#14807=CARTESIAN_POINT('Ctrl Pts',(15.8,-10.2357659846983,-10.1335518448686));
#14808=CARTESIAN_POINT('Origin',(15.8,-9.70545143020505,-11.5149238208745));
#14809=CARTESIAN_POINT('Ctrl Pts',(10.0502525316942,-9.86553218952113,-4.29750123086779));
#14810=CARTESIAN_POINT('Ctrl Pts',(11.9668350211294,-11.2772850923971,-5.98055897313701));
#14811=CARTESIAN_POINT('Ctrl Pts',(13.8834175105647,-12.689037995273,-7.66361671540623));
#14812=CARTESIAN_POINT('Ctrl Pts',(15.8,-14.1007908981489,-9.34667445767544));
#14813=CARTESIAN_POINT('Ctrl Pts',(10.0502525316942,-9.92430165934405,-4.02946472694721));
#14814=CARTESIAN_POINT('Ctrl Pts',(11.9668350211294,-11.3702854403574,-5.67542688932036));
#14815=CARTESIAN_POINT('Ctrl Pts',(13.8834175105647,-12.8166324188796,-7.32120731702056));
#14816=CARTESIAN_POINT('Ctrl Pts',(15.8,-14.262616199893,-8.96716947939371));
#14817=CARTESIAN_POINT('Ctrl Pts',(10.0502525316942,-9.97045860619055,-3.61211062987325));
#14818=CARTESIAN_POINT('Ctrl Pts',(11.9668350211295,-11.4635526451079,-5.19299729643612));
#14819=CARTESIAN_POINT('Ctrl Pts',(13.8834175105647,-12.956112555571,-6.77411605990067));
#14820=CARTESIAN_POINT('Ctrl Pts',(15.8,-14.4492065944883,-8.35500272646354));
#14821=CARTESIAN_POINT('Ctrl Pts',(10.0502525316942,-9.86609404202411,-3.40259706500424));
#14822=CARTESIAN_POINT('Ctrl Pts',(11.9668350211295,-11.3629139742223,-4.93192196434907));
#14823=CARTESIAN_POINT('Ctrl Pts',(13.8834175105647,-12.8596985741914,-6.46129704742022));
#14824=CARTESIAN_POINT('Ctrl Pts',(15.8,-14.3565185063897,-7.99062194676505));
#14825=CARTESIAN_POINT('Ctrl Pts',(10.0502525316942,-9.77087387154056,-3.30601090928165));
#14826=CARTESIAN_POINT('Ctrl Pts',(11.9668350211295,-11.2600017151874,-4.80688444200922));
#14827=CARTESIAN_POINT('Ctrl Pts',(13.8834175105647,-12.7494883087275,-6.30755492143114));
#14828=CARTESIAN_POINT('Ctrl Pts',(15.8,-14.2386161523743,-7.80842845415871));
#14829=CARTESIAN_POINT('Ctrl Pts',(10.0502525316942,-9.70530494967552,-3.24522078037662));
#14830=CARTESIAN_POINT('Ctrl Pts',(11.9668350211295,-11.1883166806212,-4.72781700580775));
#14831=CARTESIAN_POINT('Ctrl Pts',(13.8834175105647,-12.6715703878316,-6.2103780406105));
#14832=CARTESIAN_POINT('Ctrl Pts',(15.8,-14.1545821187772,-7.69297426604162));
#14833=CARTESIAN_POINT('Ctrl Pts',(10.0502525316942,-9.59290229251197,-3.13558852137589));
#14834=CARTESIAN_POINT('Ctrl Pts',(11.9668350211294,-11.0646742694967,-4.58744122478928));
#14835=CARTESIAN_POINT('Ctrl Pts',(13.8834175105647,-12.5366026187688,-6.03905717649217));
#14836=CARTESIAN_POINT('Ctrl Pts',(15.8,-14.0083745957535,-7.49090987990556));
#14837=CARTESIAN_POINT('Ctrl Pts',(10.0502525316942,-9.413101520256,-2.92757116168118));
#14838=CARTESIAN_POINT('Ctrl Pts',(11.9668350211295,-10.8702564567215,-4.32424671627921));
#14839=CARTESIAN_POINT('Ctrl Pts',(13.8834175105647,-12.3275956094625,-5.72097159497833));
#14840=CARTESIAN_POINT('Ctrl Pts',(15.8,-13.784750545928,-7.11764714957635));
#14841=CARTESIAN_POINT('Ctrl Pts',(10.0502525316942,-9.19740926566326,-2.7889486257146));
#14842=CARTESIAN_POINT('Ctrl Pts',(11.9668350211294,-10.6275127538178,-4.13765656795515));
#14843=CARTESIAN_POINT('Ctrl Pts',(13.8834175105647,-12.0577280234798,-5.48632659127459));
#14844=CARTESIAN_POINT('Ctrl Pts',(15.8,-13.4878315116343,-6.83503453351514));
#14845=CARTESIAN_POINT('Ctrl Pts',(10.0502525316942,-8.97469639188219,-2.6831512960299));
#14846=CARTESIAN_POINT('Ctrl Pts',(11.9668350211294,-10.3719655284903,-3.99115284441713));
#14847=CARTESIAN_POINT('Ctrl Pts',(13.8834175105648,-11.7692966119438,-5.29909475352163));
#14848=CARTESIAN_POINT('Ctrl Pts',(15.8,-13.1665657485518,-6.60709630190887));
#14849=CARTESIAN_POINT('Ctrl Pts',(10.0502525316942,-8.85625319397989,-2.64958522759923));
#14850=CARTESIAN_POINT('Ctrl Pts',(11.9668350211294,-10.2341088589535,-3.93994688562079));
#14851=CARTESIAN_POINT('Ctrl Pts',(13.8834175105647,-11.612095695752,-5.23040962052305));
#14852=CARTESIAN_POINT('Ctrl Pts',(15.8,-12.9899513607256,-6.52077127854461));
#14853=CARTESIAN_POINT('Ctrl Pts',(10.0502525316942,-8.77492596468499,-2.63468906623289));
#14854=CARTESIAN_POINT('Ctrl Pts',(11.9668350211294,-10.1386945339445,-3.91464433600868));
#14855=CARTESIAN_POINT('Ctrl Pts',(13.8834175105647,-11.5024631032041,-5.19459960578446));
#14856=CARTESIAN_POINT('Ctrl Pts',(15.8,-12.8662316724636,-6.47455487556025));
#14857=CARTESIAN_POINT('Ctrl Pts',(15.8,-12.9067253609027,-6.49019400603777));
#14858=CARTESIAN_POINT('Ctrl Pts',(15.8,-12.8986734787776,-6.48698118307512));
#14859=CARTESIAN_POINT('Ctrl Pts',(15.8,-12.890598163633,-6.48381086865141));
#14860=CARTESIAN_POINT('Ctrl Pts',(15.8,-12.8824994218701,-6.48068305016014));
#14861=CARTESIAN_POINT('Ctrl Pts',(15.8,-12.874377258079,-6.47759771920651));
#14862=CARTESIAN_POINT('Ctrl Pts',(15.8,-12.8662316724636,-6.47455487556025));
#14863=CARTESIAN_POINT('Origin',(15.8,-12.7887399758658,-7.95219390447097));
#14864=CARTESIAN_POINT('Ctrl Pts',(10.0502525316942,-10.7106795892491,-1.03854944428814));
#14865=CARTESIAN_POINT('Ctrl Pts',(11.9668350211294,-12.5734298318033,-2.20297683852746));
#14866=CARTESIAN_POINT('Ctrl Pts',(13.8834175105647,-14.4361800743576,-3.36740423276678));
#14867=CARTESIAN_POINT('Ctrl Pts',(15.8,-16.2989303169119,-4.5318316270061));
#14868=CARTESIAN_POINT('Ctrl Pts',(10.0502525316942,-10.6837448416591,-0.765470815703814));
#14869=CARTESIAN_POINT('Ctrl Pts',(11.9668350211294,-12.5675874193204,-1.88404029388038));
#14870=CARTESIAN_POINT('Ctrl Pts',(13.8834175105647,-14.4517192592367,-3.00232469790949));
#14871=CARTESIAN_POINT('Ctrl Pts',(15.8,-16.335561836898,-4.12089417608606));
#14872=CARTESIAN_POINT('Ctrl Pts',(10.0502525316942,-10.5986742216641,-0.354275884655604));
#14873=CARTESIAN_POINT('Ctrl Pts',(11.9668350211294,-12.5072118829665,-1.39639701818897));
#14874=CARTESIAN_POINT('Ctrl Pts',(13.8834175105647,-14.4153151096236,-2.43890221878171));
#14875=CARTESIAN_POINT('Ctrl Pts',(15.8,-16.3238527709261,-3.48102335231507));
#14876=CARTESIAN_POINT('Ctrl Pts',(10.0502525316942,-10.4346757823309,-0.187261072828499));
#14877=CARTESIAN_POINT('Ctrl Pts',(11.9668350211294,-12.3308235163868,-1.17919268731443));
#14878=CARTESIAN_POINT('Ctrl Pts',(13.8834175105647,-14.2269575174279,-2.17117887432506));
#14879=CARTESIAN_POINT('Ctrl Pts',(15.8,-16.1231052514838,-3.16311048881098));
#14880=CARTESIAN_POINT('Ctrl Pts',(10.0502525316942,-10.3142698682631,-0.124824203483033));
#14881=CARTESIAN_POINT('Ctrl Pts',(11.9668350211295,-12.1943100355803,-1.09207394643473));
#14882=CARTESIAN_POINT('Ctrl Pts',(13.8834175105647,-14.0746341437949,-2.05901454824881));
#14883=CARTESIAN_POINT('Ctrl Pts',(15.8,-15.9546743111121,-3.02626429120051));
#14884=CARTESIAN_POINT('Ctrl Pts',(10.0502525316942,-10.2331249635989,-0.0872711810328558));
#14885=CARTESIAN_POINT('Ctrl Pts',(11.9668350211294,-12.1017003635113,-1.03902815454411));
#14886=CARTESIAN_POINT('Ctrl Pts',(13.8834175105647,-13.9705005205662,-1.99067177195527));
#14887=CARTESIAN_POINT('Ctrl Pts',(15.8,-15.8390759204785,-2.94242874546653));
#14888=CARTESIAN_POINT('Ctrl Pts',(10.0502525316942,-10.09234540735,-0.0177390798696546));
#14889=CARTESIAN_POINT('Ctrl Pts',(11.9668350211294,-11.9407308952458,-0.943730501418607));
#14890=CARTESIAN_POINT('Ctrl Pts',(13.8834175105647,-13.789197555515,-1.86944300220407));
#14891=CARTESIAN_POINT('Ctrl Pts',(15.8,-15.6375830434108,-2.79543442375303));
#14892=CARTESIAN_POINT('Ctrl Pts',(10.0502525316942,-9.85706386916291,0.124535428292433));
#14893=CARTESIAN_POINT('Ctrl Pts',(11.9668350211294,-11.6744970487389,-0.753496320252986));
#14894=CARTESIAN_POINT('Ctrl Pts',(13.8834175105647,-13.4921256030567,-1.63151416409049));
#14895=CARTESIAN_POINT('Ctrl Pts',(15.8,-15.3095587826327,-2.50954591263591));
#14896=CARTESIAN_POINT('Ctrl Pts',(10.0502525316942,-9.60909091476054,0.189717758784556));
#14897=CARTESIAN_POINT('Ctrl Pts',(11.9668350211294,-11.3859738307471,-0.651053436707714));
#14898=CARTESIAN_POINT('Ctrl Pts',(13.8834175105647,-13.1629551482145,-1.49175101418762));
#14899=CARTESIAN_POINT('Ctrl Pts',(15.8,-14.9398380642011,-2.33252220967989));
#14900=CARTESIAN_POINT('Ctrl Pts',(10.0502525316942,-9.36458479377687,0.221513186022213));
#14901=CARTESIAN_POINT('Ctrl Pts',(11.9668350211294,-11.0976614182865,-0.590690300968109));
#14902=CARTESIAN_POINT('Ctrl Pts',(13.8834175105648,-12.8307816497324,-1.40281548080796));
#14903=CARTESIAN_POINT('Ctrl Pts',(15.8,-14.563858274242,-2.21501896779828));
#14904=CARTESIAN_POINT('Ctrl Pts',(10.0502525316942,-9.24156417346731,0.21682744723956));
#14905=CARTESIAN_POINT('Ctrl Pts',(11.9668350211294,-10.9507264633732,-0.584598599726619));
#14906=CARTESIAN_POINT('Ctrl Pts',(13.8834175105647,-12.6600447395717,-1.38608024219576));
#14907=CARTESIAN_POINT('Ctrl Pts',(15.8,-14.3692070294775,-2.18750628916194));
#14908=CARTESIAN_POINT('Ctrl Pts',(10.0502525316942,-9.15961421508102,0.205863042617261));
#14909=CARTESIAN_POINT('Ctrl Pts',(11.9668350211294,-10.8521631299943,-0.590019092973716));
#14910=CARTESIAN_POINT('Ctrl Pts',(13.8834175105647,-12.5447120449076,-1.38590122856469));
#14911=CARTESIAN_POINT('Ctrl Pts',(15.8,-14.2372609598209,-2.18178336415567));
#14912=CARTESIAN_POINT('Ctrl Pts',(15.8,-14.2806055031745,-2.18414382321291));
#14913=CARTESIAN_POINT('Ctrl Pts',(15.8,-14.2719548913156,-2.18357641541193));
#14914=CARTESIAN_POINT('Ctrl Pts',(15.8,-14.2632951291918,-2.18305667683517));
#14915=CARTESIAN_POINT('Ctrl Pts',(15.8,-14.2546262189952,-2.18258459351507));
#14916=CARTESIAN_POINT('Ctrl Pts',(15.8,-14.2459481624974,-2.18216015604921));
#14917=CARTESIAN_POINT('Ctrl Pts',(15.8,-14.2372609598209,-2.18178336415567));
#14918=CARTESIAN_POINT('Origin',(15.8,-14.6201775482978,-3.61104784250494));
#14919=CARTESIAN_POINT('Ctrl Pts',(10.0502525316942,-10.5073910450885,2.32206279789789));
#14920=CARTESIAN_POINT('Ctrl Pts',(11.1454425256572,-11.7253388222013,2.01816863800157));
#14921=CARTESIAN_POINT('Ctrl Pts',(12.3775312688656,-13.0955300714531,1.67628770811821));
#14922=CARTESIAN_POINT('Ctrl Pts',(13.7465187613193,-14.617964792844,1.29642000824781));
#14923=CARTESIAN_POINT('Ctrl Pts',(14.2941137583009,-15.2269386814004,1.14447292829964));
#14924=CARTESIAN_POINT('Ctrl Pts',(14.8417087552824,-15.8359125699568,0.992525848351483));
#14925=CARTESIAN_POINT('Ctrl Pts',(15.3208543776412,-16.3687647224436,0.859572153396841));
#14926=CARTESIAN_POINT('Ctrl Pts',(15.5946518761319,-16.6732516667218,0.783598613422761));
#14927=CARTESIAN_POINT('Ctrl Pts',(15.7315506253773,-16.8254951388609,0.745611843435721));
#14928=CARTESIAN_POINT('Ctrl Pts',(15.8,-16.9016168749304,0.7266184584422));
#14929=CARTESIAN_POINT('Ctrl Pts',(10.0502525316942,-10.3973886408451,2.57345271232945));
#14930=CARTESIAN_POINT('Ctrl Pts',(11.1454425256572,-11.618687280661,2.29815463811993));
#14931=CARTESIAN_POINT('Ctrl Pts',(12.3775312688656,-12.9928273987101,1.98887116228557));
#14932=CARTESIAN_POINT('Ctrl Pts',(13.7465187613193,-14.519468077176,1.64478997784958));
#14933=CARTESIAN_POINT('Ctrl Pts',(14.2941137583009,-15.1301263986154,1.50716238874916));
#14934=CARTESIAN_POINT('Ctrl Pts',(14.8417087552824,-15.740805777741,1.36958497392712));
#14935=CARTESIAN_POINT('Ctrl Pts',(15.3208543776412,-16.2751437253593,1.24918922664557));
#14936=CARTESIAN_POINT('Ctrl Pts',(15.5946518761319,-16.5804716520035,1.18037249165619));
#14937=CARTESIAN_POINT('Ctrl Pts',(15.7315506253773,-16.7331376997671,1.14596909077302));
#14938=CARTESIAN_POINT('Ctrl Pts',(15.8,-16.8094688647556,1.12876296113493));
#14939=CARTESIAN_POINT('Ctrl Pts',(10.0502525316942,-10.189368118401,2.93870070814822));
#14940=CARTESIAN_POINT('Ctrl Pts',(11.1454425256572,-11.4106316171747,2.70946206711307));
#14941=CARTESIAN_POINT('Ctrl Pts',(12.3775312688656,-12.7843360022416,2.45105312324518));
#14942=CARTESIAN_POINT('Ctrl Pts',(13.7465187613194,-14.310894320163,2.16445481731473));
#14943=CARTESIAN_POINT('Ctrl Pts',(14.2941137583009,-14.9215151635443,2.04980959621707));
#14944=CARTESIAN_POINT('Ctrl Pts',(14.8417087552824,-15.5321104940175,1.93510378473096));
#14945=CARTESIAN_POINT('Ctrl Pts',(15.3208543776412,-16.0663892944466,1.83475492870443));
#14946=CARTESIAN_POINT('Ctrl Pts',(15.5946518761319,-16.3717012113088,1.77743586902584));
#14947=CARTESIAN_POINT('Ctrl Pts',(15.7315506253773,-16.5243546442885,1.7487703415134));
#14948=CARTESIAN_POINT('Ctrl Pts',(15.8,-16.6006836129618,1.7344429264487));
#14949=CARTESIAN_POINT('Ctrl Pts',(10.0502525316942,-9.95881139224219,3.05808383535426));
#14950=CARTESIAN_POINT('Ctrl Pts',(11.1454425256572,-11.1626816238278,2.85649631904974));
#14951=CARTESIAN_POINT('Ctrl Pts',(12.3775312688656,-12.5171248305866,2.62997738853437));
#14952=CARTESIAN_POINT('Ctrl Pts',(13.7465187613193,-14.0219712727573,2.37801889657081));
#14953=CARTESIAN_POINT('Ctrl Pts',(14.2941137583008,-14.6239108703276,2.27723855544496));
#14954=CARTESIAN_POINT('Ctrl Pts',(14.8417087552823,-15.225860952321,2.17648960137063));
#14955=CARTESIAN_POINT('Ctrl Pts',(15.3208543776412,-15.7525640332375,2.08832456454097));
#14956=CARTESIAN_POINT('Ctrl Pts',(15.5946518761319,-16.0535332175881,2.03793255455515));
#14957=CARTESIAN_POINT('Ctrl Pts',(15.7315506253773,-16.2040188475872,2.01273965647872));
#14958=CARTESIAN_POINT('Ctrl Pts',(15.8,-16.2792607370613,2.00014043670969));
#14959=CARTESIAN_POINT('Ctrl Pts',(10.0502525316942,-9.78147886731912,3.07559947603193));
#14960=CARTESIAN_POINT('Ctrl Pts',(11.1454425256572,-10.9672359168267,2.88676320881926));
#14961=CARTESIAN_POINT('Ctrl Pts',(12.3775312688656,-12.3013551830101,2.67450622091511));
#14962=CARTESIAN_POINT('Ctrl Pts',(13.7465187613194,-13.7835653267336,2.43847871808159));
#14963=CARTESIAN_POINT('Ctrl Pts',(14.2941137583009,-14.3764510158762,2.34406982037812));
#14964=CARTESIAN_POINT('Ctrl Pts',(14.8417087552824,-14.9693534649946,2.2496825286364));
#14965=CARTESIAN_POINT('Ctrl Pts',(15.3208543776412,-15.4881379273167,2.16708696976892));
#14966=CARTESIAN_POINT('Ctrl Pts',(15.5946518761319,-15.7845797896778,2.11988125471031));
#14967=CARTESIAN_POINT('Ctrl Pts',(15.7315506253773,-15.9328023798814,2.09628053589475));
#14968=CARTESIAN_POINT('Ctrl Pts',(15.8,-16.0069121954757,2.08447826919396));
#14969=CARTESIAN_POINT('Ctrl Pts',(10.0502525316942,-9.60383008034201,3.1022368453188));
#14970=CARTESIAN_POINT('Ctrl Pts',(11.1454425256572,-10.7718807970721,2.92542368552957));
#14971=CARTESIAN_POINT('Ctrl Pts',(12.3775312688656,-12.0859609655105,2.72674232124834));
#14972=CARTESIAN_POINT('Ctrl Pts',(13.7465187613193,-13.5460266034681,2.5057485169523));
#14973=CARTESIAN_POINT('Ctrl Pts',(14.2941137583008,-14.1300531231308,2.41735366657091));
#14974=CARTESIAN_POINT('Ctrl Pts',(14.8417087552824,-14.7140823594691,2.32898625556579));
#14975=CARTESIAN_POINT('Ctrl Pts',(15.3208543776412,-15.2251071015168,2.25165628918294));
#14976=CARTESIAN_POINT('Ctrl Pts',(15.5946518761319,-15.5171202021386,2.20745725592095));
#14977=CARTESIAN_POINT('Ctrl Pts',(15.7315506253773,-15.6631270213657,2.18536045543708));
#14978=CARTESIAN_POINT('Ctrl Pts',(15.8,-15.7361301911613,2.17430963295026));
#14979=CARTESIAN_POINT('Ctrl Pts',(10.0502525316942,-9.33616641898042,3.1641697547985));
#14980=CARTESIAN_POINT('Ctrl Pts',(11.1454425256572,-10.4789053528453,3.00789330574878));
#14981=CARTESIAN_POINT('Ctrl Pts',(12.3775312688656,-11.7645911992084,2.83212323706007));
#14982=CARTESIAN_POINT('Ctrl Pts',(13.7465187613193,-13.1930250082462,2.6367816468882));
#14983=CARTESIAN_POINT('Ctrl Pts',(14.2941137583008,-13.7643997282132,2.55864547926933));
#14984=CARTESIAN_POINT('Ctrl Pts',(14.8417087552823,-14.3357867368398,2.48051412346291));
#14985=CARTESIAN_POINT('Ctrl Pts',(15.3208543776412,-14.8357465708549,2.4121476997586));
#14986=CARTESIAN_POINT('Ctrl Pts',(15.5946518761319,-15.1214332106675,2.37307933395524));
#14987=CARTESIAN_POINT('Ctrl Pts',(15.7315506253773,-15.2642777469938,2.35354562736142));
#14988=CARTESIAN_POINT('Ctrl Pts',(15.8,-15.3356989303604,2.34377834929581));
#14989=CARTESIAN_POINT('Ctrl Pts',(10.0502525316942,-9.08015411140624,3.14987939962279));
#14990=CARTESIAN_POINT('Ctrl Pts',(11.1454425256572,-10.19428901683,3.0067293155267));
#14991=CARTESIAN_POINT('Ctrl Pts',(12.3775312688656,-11.4477380681646,2.84574388114627));
#14992=CARTESIAN_POINT('Ctrl Pts',(13.7465187613193,-12.8404112867165,2.66681194224705));
#14993=CARTESIAN_POINT('Ctrl Pts',(14.2941137583008,-13.3974811152093,2.59523983509501));
#14994=CARTESIAN_POINT('Ctrl Pts',(14.8417087552823,-13.9545565014729,2.52367459367682));
#14995=CARTESIAN_POINT('Ctrl Pts',(15.3208543776412,-14.4419957464975,2.46105288517697));
#14996=CARTESIAN_POINT('Ctrl Pts',(15.5946518761319,-14.7205303350335,2.42526642923796));
#14997=CARTESIAN_POINT('Ctrl Pts',(15.7315506253773,-14.8597981794497,2.40737388088825));
#14998=CARTESIAN_POINT('Ctrl Pts',(15.8,-14.9294316110386,2.39842700063224));
#14999=CARTESIAN_POINT('Ctrl Pts',(10.0502525316942,-8.83780343943476,3.10442465522081));
#15000=CARTESIAN_POINT('Ctrl Pts',(11.1454425256572,-9.92307916160989,2.96904269314958));
#15001=CARTESIAN_POINT('Ctrl Pts',(12.3775312688656,-11.1440266947135,2.81681208487056));
#15002=CARTESIAN_POINT('Ctrl Pts',(13.7465187613194,-12.5006225450517,2.64759182043347));
#15003=CARTESIAN_POINT('Ctrl Pts',(14.2941137583009,-13.0432610264625,2.57990456259871));
#15004=CARTESIAN_POINT('Ctrl Pts',(14.8417087552824,-13.585900959023,2.51222601461465));
#15005=CARTESIAN_POINT('Ctrl Pts',(15.3208543776412,-14.0607104514503,2.45300459283688));
#15006=CARTESIAN_POINT('Ctrl Pts',(15.594651876132,-14.3320296071118,2.41916045348293));
#15007=CARTESIAN_POINT('Ctrl Pts',(15.7315506253773,-14.4676893285877,2.40223924596973));
#15008=CARTESIAN_POINT('Ctrl Pts',(15.8,-14.5355190612237,2.39377787334028));
#15009=CARTESIAN_POINT('Ctrl Pts',(10.0502525316942,-8.72224646189196,3.06201554081689));
#15010=CARTESIAN_POINT('Ctrl Pts',(11.1454425256572,-9.79262845293104,2.92828468444751));
#15011=CARTESIAN_POINT('Ctrl Pts',(12.3775312688656,-10.9969124481398,2.77780914227504));
#15012=CARTESIAN_POINT('Ctrl Pts',(13.7465187613193,-12.3349000504671,2.61064282371592));
#15013=CARTESIAN_POINT('Ctrl Pts',(14.2941137583009,-12.870096284426,2.54377597211689));
#15014=CARTESIAN_POINT('Ctrl Pts',(14.8417087552824,-13.4053047729009,2.47690579066087));
#15015=CARTESIAN_POINT('Ctrl Pts',(15.3208543776412,-13.8736084123374,2.41839541117503));
#15016=CARTESIAN_POINT('Ctrl Pts',(15.5946518761319,-14.1412058111469,2.38496218052016));
#15017=CARTESIAN_POINT('Ctrl Pts',(15.7315506253773,-14.2750057235919,2.3682452355795));
#15018=CARTESIAN_POINT('Ctrl Pts',(15.8,-14.3419045980318,2.35988705705641));
#15019=CARTESIAN_POINT('Ctrl Pts',(10.0502525316942,-8.64769560732005,3.02626384252387));
#15020=CARTESIAN_POINT('Ctrl Pts',(11.1454425256572,-9.70806748165927,2.89260526381666));
#15021=CARTESIAN_POINT('Ctrl Pts',(12.3775312688656,-10.9009858402909,2.74223936277106));
#15022=CARTESIAN_POINT('Ctrl Pts',(13.7465187613193,-12.2264506832149,2.57516613938705));
#15023=CARTESIAN_POINT('Ctrl Pts',(14.2941137583009,-12.7566366203845,2.50833685003344));
#15024=CARTESIAN_POINT('Ctrl Pts',(14.8417087552824,-13.2868225575541,2.44150756067984));
#15025=CARTESIAN_POINT('Ctrl Pts',(15.3208543776412,-13.7507352525775,2.38303193249543));
#15026=CARTESIAN_POINT('Ctrl Pts',(15.5946518761319,-14.0158282211623,2.34961728781863));
#15027=CARTESIAN_POINT('Ctrl Pts',(15.7315506253773,-14.1483747054547,2.33290996548023));
#15028=CARTESIAN_POINT('Ctrl Pts',(15.8,-14.2146479476009,2.32455630431103));
#15029=CARTESIAN_POINT('Ctrl Pts',(15.8,-14.2566004799664,2.33570557485288));
#15030=CARTESIAN_POINT('Ctrl Pts',(15.8,-14.2481979205348,2.33357202566325));
#15031=CARTESIAN_POINT('Ctrl Pts',(15.8,-14.2398013892846,2.33139031275994));
#15032=CARTESIAN_POINT('Ctrl Pts',(15.8,-14.2314108839843,2.32916045010432));
#15033=CARTESIAN_POINT('Ctrl Pts',(15.8,-14.2230264034132,2.32688244718599));
#15034=CARTESIAN_POINT('Ctrl Pts',(15.8,-14.2146479476009,2.32455630431103));
#15035=CARTESIAN_POINT('Origin',(15.8,-15.0204902775358,1.08357274193521));
#15036=CARTESIAN_POINT('Ctrl Pts',(10.0502525316942,-9.2755658561365,5.45537535466284));
#15037=CARTESIAN_POINT('Ctrl Pts',(11.1454425256572,-10.527811485966,5.54272139501843));
#15038=CARTESIAN_POINT('Ctrl Pts',(12.3775312688656,-11.9365878195243,5.64098569041847));
#15039=CARTESIAN_POINT('Ctrl Pts',(13.7465187613193,-13.5018948568112,5.75016824086296));
#15040=CARTESIAN_POINT('Ctrl Pts',(14.2941137583009,-14.1280176717259,5.79384126104075));
#15041=CARTESIAN_POINT('Ctrl Pts',(14.8417087552824,-14.7541404866407,5.83751428121855));
#15042=CARTESIAN_POINT('Ctrl Pts',(15.3208543776412,-15.3019979496911,5.87572817387412));
#15043=CARTESIAN_POINT('Ctrl Pts',(15.5946518761319,-15.6150593571485,5.89756468396302));
#15044=CARTESIAN_POINT('Ctrl Pts',(15.7315506253773,-15.7715900608772,5.90848293900746));
#15045=CARTESIAN_POINT('Ctrl Pts',(15.8,-15.8498554127416,5.91394206652969));
#15046=CARTESIAN_POINT('Ctrl Pts',(10.0502525316942,-9.09326359699885,5.66046875858054));
#15047=CARTESIAN_POINT('Ctrl Pts',(11.1454425256572,-10.3398594101876,5.77604676609019));
#15048=CARTESIAN_POINT('Ctrl Pts',(12.3775312688656,-11.7423187718539,5.90654052031257));
#15049=CARTESIAN_POINT('Ctrl Pts',(13.7465187613193,-13.3005670731329,6.05105541408884));
#15050=CARTESIAN_POINT('Ctrl Pts',(14.2941137583009,-13.9238668895967,6.10886731837785));
#15051=CARTESIAN_POINT('Ctrl Pts',(14.8417087552824,-14.5471710567224,6.16673138983645));
#15052=CARTESIAN_POINT('Ctrl Pts',(15.3208543776412,-15.0925608480023,6.21734620559881));
#15053=CARTESIAN_POINT('Ctrl Pts',(15.5946518761319,-15.4042104768461,6.24624880770452));
#15054=CARTESIAN_POINT('Ctrl Pts',(15.7315506253773,-15.5600357233504,6.26070528969669));
#15055=CARTESIAN_POINT('Ctrl Pts',(15.8,-15.6379479616747,6.26792891516604));
#15056=CARTESIAN_POINT('Ctrl Pts',(10.0502525316942,-8.78255765938311,5.94355560685309));
#15057=CARTESIAN_POINT('Ctrl Pts',(11.1454425256572,-10.0148869038525,6.10292787924083));
#15058=CARTESIAN_POINT('Ctrl Pts',(12.3775312688656,-11.4012092316412,6.2816544949474));
#15059=CARTESIAN_POINT('Ctrl Pts',(13.7465187613194,-12.9416164381759,6.48081852219944));
#15060=CARTESIAN_POINT('Ctrl Pts',(14.2941137583009,-13.5577787105922,6.56047693355264));
#15061=CARTESIAN_POINT('Ctrl Pts',(14.8417087552824,-14.1739356301478,6.64007218801815));
#15062=CARTESIAN_POINT('Ctrl Pts',(15.3208543776412,-14.7130746018355,6.70973770503938));
#15063=CARTESIAN_POINT('Ctrl Pts',(15.594651876132,-15.0211560817903,6.74957096648566));
#15064=CARTESIAN_POINT('Ctrl Pts',(15.7315506253773,-15.1751962901528,6.76948132483471));
#15065=CARTESIAN_POINT('Ctrl Pts',(15.8,-15.2522168679322,6.77944209185894));
#15066=CARTESIAN_POINT('Ctrl Pts',(10.0502525316942,-8.52639512605652,5.98584659003549));
#15067=CARTESIAN_POINT('Ctrl Pts',(11.1454425256572,-9.73363772297167,6.16614182963237));
#15068=CARTESIAN_POINT('Ctrl Pts',(12.3775312688656,-11.0917875706281,6.36925721416675));
#15069=CARTESIAN_POINT('Ctrl Pts',(13.7465187613193,-12.6008409910269,6.59465188812854));
#15070=CARTESIAN_POINT('Ctrl Pts',(14.2941137583008,-13.2044623836355,6.68481335297615));
#15071=CARTESIAN_POINT('Ctrl Pts',(14.8417087552823,-13.8080839907189,6.77500635669625));
#15072=CARTESIAN_POINT('Ctrl Pts',(15.3208543776412,-14.3362528301216,6.85391541259334));
#15073=CARTESIAN_POINT('Ctrl Pts',(15.5946518761319,-14.6380635126529,6.89899411967348));
#15074=CARTESIAN_POINT('Ctrl Pts',(15.7315506253773,-14.7889688752189,6.92153660547059));
#15075=CARTESIAN_POINT('Ctrl Pts',(15.8,-14.8644215375261,6.9328050579454));
#15076=CARTESIAN_POINT('Ctrl Pts',(10.0502525316942,-8.35233000922534,5.94770436886828));
#15077=CARTESIAN_POINT('Ctrl Pts',(11.1454425256572,-9.5384055936255,6.13452948592056));
#15078=CARTESIAN_POINT('Ctrl Pts',(12.3775312688656,-10.8728200811769,6.34492663085593));
#15079=CARTESIAN_POINT('Ctrl Pts',(13.7465187613193,-12.3554217499083,6.57847782979355));
#15080=CARTESIAN_POINT('Ctrl Pts',(14.2941137583008,-12.9484634259519,6.67190108779269));
#15081=CARTESIAN_POINT('Ctrl Pts',(14.8417087552824,-13.541513949349,6.76534871907581));
#15082=CARTESIAN_POINT('Ctrl Pts',(15.3208543776412,-14.0604304019321,6.84710780571679));
#15083=CARTESIAN_POINT('Ctrl Pts',(15.5946518761319,-14.3569506718,6.89381786952799));
#15084=CARTESIAN_POINT('Ctrl Pts',(15.7315506253773,-14.5052116854016,6.91717532204614));
#15085=CARTESIAN_POINT('Ctrl Pts',(15.8,-14.5793414094266,6.92885189186191));
#15086=CARTESIAN_POINT('Ctrl Pts',(10.0502525316942,-8.1751443698686,5.91814205125966));
#15087=CARTESIAN_POINT('Ctrl Pts',(11.1454425256572,-9.34066488658195,6.11093026523681));
#15088=CARTESIAN_POINT('Ctrl Pts',(12.3775312688656,-10.6518240329443,6.32804641946555));
#15089=CARTESIAN_POINT('Ctrl Pts',(13.7465187613193,-12.1087200255634,6.56905244176938));
#15090=CARTESIAN_POINT('Ctrl Pts',(14.2941137583008,-12.6914777697296,6.66545776271567));
#15091=CARTESIAN_POINT('Ctrl Pts',(14.8417087552823,-13.2742297865971,6.76188862893655));
#15092=CARTESIAN_POINT('Ctrl Pts',(15.3208543776412,-13.7841395850464,6.84625768114735));
#15093=CARTESIAN_POINT('Ctrl Pts',(15.5946518761319,-14.0755188249216,6.89445870116997));
#15094=CARTESIAN_POINT('Ctrl Pts',(15.7315506253773,-14.2212078760573,6.9185617481891));
#15095=CARTESIAN_POINT('Ctrl Pts',(15.8,-14.2940529083518,6.93061101156267));
#15096=CARTESIAN_POINT('Ctrl Pts',(10.0502525316942,-7.90144264462466,5.8943312499999));
#15097=CARTESIAN_POINT('Ctrl Pts',(11.1454425256572,-9.03654403267794,6.09882926548584));
#15098=CARTESIAN_POINT('Ctrl Pts',(12.3775312688656,-10.3136205759385,6.32895925304843));
#15099=CARTESIAN_POINT('Ctrl Pts',(13.7465187613193,-11.7325052253954,6.58458807992399));
#15100=CARTESIAN_POINT('Ctrl Pts',(14.2941137583008,-12.3000601956136,6.68684049565601));
#15101=CARTESIAN_POINT('Ctrl Pts',(14.8417087552823,-12.86762490695,6.7891006747503));
#15102=CARTESIAN_POINT('Ctrl Pts',(15.3208543776411,-13.364240995629,6.87857591366296));
#15103=CARTESIAN_POINT('Ctrl Pts',(15.5946518761319,-13.6480178551891,6.92970162298621));
#15104=CARTESIAN_POINT('Ctrl Pts',(15.7315506253773,-13.7899072524002,6.95526524865974));
#15105=CARTESIAN_POINT('Ctrl Pts',(15.8,-13.8608510891535,6.96804637462761));
#15106=CARTESIAN_POINT('Ctrl Pts',(10.0502525316942,-7.66237562613099,5.80163007173558));
#15107=CARTESIAN_POINT('Ctrl Pts',(11.1454425256572,-8.76621669669801,6.00977287125004));
#15108=CARTESIAN_POINT('Ctrl Pts',(12.3775312688656,-10.008064757174,6.24400287259235));
#15109=CARTESIAN_POINT('Ctrl Pts',(13.7465187613193,-11.3878685250288,6.50418764618811));
#15110=CARTESIAN_POINT('Ctrl Pts',(14.2941137583008,-11.9397903730643,6.60826243593386));
#15111=CARTESIAN_POINT('Ctrl Pts',(14.8417087552823,-12.4917152115347,6.71234494803684));
#15112=CARTESIAN_POINT('Ctrl Pts',(15.3208543776411,-12.9746485138656,6.80341474110257));
#15113=CARTESIAN_POINT('Ctrl Pts',(15.5946518761319,-13.2506092458454,6.85545164006593));
#15114=CARTESIAN_POINT('Ctrl Pts',(15.7315506253773,-13.388589908828,6.88147085648712));
#15115=CARTESIAN_POINT('Ctrl Pts',(15.8,-13.4575799757384,6.89447978145678));
#15116=CARTESIAN_POINT('Ctrl Pts',(10.0502525316942,-7.44593237535689,5.68351040711504));
#15117=CARTESIAN_POINT('Ctrl Pts',(11.1454425256572,-8.51992624992032,5.89012315163304));
#15118=CARTESIAN_POINT('Ctrl Pts',(12.3775312688656,-9.72815762348205,6.12263633930509));
#15119=CARTESIAN_POINT('Ctrl Pts',(13.7465187613194,-11.0706489050023,6.38090895110341));
#15120=CARTESIAN_POINT('Ctrl Pts',(14.2941137583009,-11.60764526865,6.4842189332274));
#15121=CARTESIAN_POINT('Ctrl Pts',(14.8417087552824,-12.1446403255654,6.58753713858487));
#15122=CARTESIAN_POINT('Ctrl Pts',(15.3208543776412,-12.6145114073305,6.6779380072571));
#15123=CARTESIAN_POINT('Ctrl Pts',(15.594651876132,-12.8830096730692,6.72959247024461));
#15124=CARTESIAN_POINT('Ctrl Pts',(15.7315506253773,-13.0172586761616,6.755420518422));
#15125=CARTESIAN_POINT('Ctrl Pts',(15.8,-13.0843832933218,6.76833381495438));
#15126=CARTESIAN_POINT('Ctrl Pts',(10.0502525316942,-7.34913449516209,5.60747221894231));
#15127=CARTESIAN_POINT('Ctrl Pts',(11.1454425256572,-8.40845336995523,5.81105284226644));
#15128=CARTESIAN_POINT('Ctrl Pts',(12.3775312688656,-9.60029668798142,6.04008639989118));
#15129=CARTESIAN_POINT('Ctrl Pts',(13.7465187613193,-10.9244551954278,6.29456266363366));
#15130=CARTESIAN_POINT('Ctrl Pts',(14.2941137583009,-11.4541199893924,6.3963532371211));
#15131=CARTESIAN_POINT('Ctrl Pts',(14.8417087552824,-11.9837969855611,6.49814440704391));
#15132=CARTESIAN_POINT('Ctrl Pts',(15.3208543776412,-12.4472605569962,6.58721149497458));
#15133=CARTESIAN_POINT('Ctrl Pts',(15.5946518761319,-12.7120921703849,6.63810674341679));
#15134=CARTESIAN_POINT('Ctrl Pts',(15.7315506253773,-12.8445091889311,6.66355442687238));
#15135=CARTESIAN_POINT('Ctrl Pts',(15.8,-12.9107166186057,6.67627821583014));
#15136=CARTESIAN_POINT('Ctrl Pts',(10.0502525316942,-7.28928030147641,5.55043285230422));
#15137=CARTESIAN_POINT('Ctrl Pts',(11.1454425256572,-8.33905665452735,5.75098891959401));
#15138=CARTESIAN_POINT('Ctrl Pts',(12.3775312688656,-9.52005505170966,5.97661449529503));
#15139=CARTESIAN_POINT('Ctrl Pts',(13.7465187613193,-10.8322754930233,6.22730957940728));
#15140=CARTESIAN_POINT('Ctrl Pts',(14.2941137583009,-11.3571636695488,6.32758761305217));
#15141=CARTESIAN_POINT('Ctrl Pts',(14.8417087552824,-11.8820518460743,6.42786564669707));
#15142=CARTESIAN_POINT('Ctrl Pts',(15.3208543776412,-12.3413290005341,6.51560892613635));
#15143=CARTESIAN_POINT('Ctrl Pts',(15.5946518761319,-12.6037730887968,6.56574794295881));
#15144=CARTESIAN_POINT('Ctrl Pts',(15.7315506253773,-12.7349951329282,6.59081745137003));
#15145=CARTESIAN_POINT('Ctrl Pts',(15.8,-12.8006061549939,6.60335220557564));
#15146=CARTESIAN_POINT('Ctrl Pts',(15.8,-12.8370600702028,6.62691983743441));
#15147=CARTESIAN_POINT('Ctrl Pts',(15.8,-12.8297280642598,6.62229417791417));
#15148=CARTESIAN_POINT('Ctrl Pts',(15.8,-12.8224166748639,6.61762457479065));
#15149=CARTESIAN_POINT('Ctrl Pts',(15.8,-12.8151258955788,6.61291104065239));
#15150=CARTESIAN_POINT('Ctrl Pts',(15.8,-12.8078557223109,6.60815358414732));
#15151=CARTESIAN_POINT('Ctrl Pts',(15.8,-12.8006061549939,6.60335220557564));
#15152=CARTESIAN_POINT('Origin',(15.8,-13.950492764499,5.67212567669951));
#15153=CARTESIAN_POINT('Ctrl Pts',(10.0502525316942,-7.13578365451838,8.05467776187827));
#15154=CARTESIAN_POINT('Ctrl Pts',(11.1454425256572,-8.29974860990865,8.52471396348012));
#15155=CARTESIAN_POINT('Ctrl Pts',(12.3775312688656,-9.6092091847227,9.05350469028219));
#15156=CARTESIAN_POINT('Ctrl Pts',(13.7465187613193,-11.0641653789605,9.6410499422845));
#15157=CARTESIAN_POINT('Ctrl Pts',(14.2941137583009,-11.6461478566557,9.87606804308543));
#15158=CARTESIAN_POINT('Ctrl Pts',(14.8417087552824,-12.2281303343508,10.1110861438864));
#15159=CARTESIAN_POINT('Ctrl Pts',(15.3208543776412,-12.737365002334,10.3167269820872));
#15160=CARTESIAN_POINT('Ctrl Pts',(15.5946518761319,-13.0283562411816,10.4342360324876));
#15161=CARTESIAN_POINT('Ctrl Pts',(15.7315506253773,-13.1738518606054,10.4929905576879));
#15162=CARTESIAN_POINT('Ctrl Pts',(15.8,-13.2465996703173,10.522367820288));
#15163=CARTESIAN_POINT('Ctrl Pts',(10.0502525316942,-6.89902655578542,8.19339868393687));
#15164=CARTESIAN_POINT('Ctrl Pts',(11.1454425256572,-8.04889405860839,8.68853919251131));
#15165=CARTESIAN_POINT('Ctrl Pts',(12.3775312688656,-9.34238794408146,9.24602752966092));
#15166=CARTESIAN_POINT('Ctrl Pts',(13.7465187613193,-10.779712402918,9.86499535005157));
#15167=CARTESIAN_POINT('Ctrl Pts',(14.2941137583009,-11.354640872798,10.1125880646808));
#15168=CARTESIAN_POINT('Ctrl Pts',(14.8417087552824,-11.9295571981554,10.3602324253388));
#15169=CARTESIAN_POINT('Ctrl Pts',(15.3208543776412,-12.4326127553978,10.5769051976768));
#15170=CARTESIAN_POINT('Ctrl Pts',(15.5946518761319,-12.7200777462785,10.7006983402633));
#15171=CARTESIAN_POINT('Ctrl Pts',(15.7315506253773,-12.8638090371883,10.7626000339661));
#15172=CARTESIAN_POINT('Ctrl Pts',(15.8,-12.9356757561148,10.793546315752));
#15173=CARTESIAN_POINT('Ctrl Pts',(10.0502525316942,-6.51604789180993,8.36661813687798));
#15174=CARTESIAN_POINT('Ctrl Pts',(11.1454425256572,-7.63881390938367,8.8990008542554));
#15175=CARTESIAN_POINT('Ctrl Pts',(12.3775312688656,-8.90205445633838,9.49738068383039));
#15176=CARTESIAN_POINT('Ctrl Pts',(13.7465187613194,-10.3055239107478,10.1628080503653));
#15177=CARTESIAN_POINT('Ctrl Pts',(14.2941137583009,-10.8669132727127,10.4289722391039));
#15178=CARTESIAN_POINT('Ctrl Pts',(14.8417087552824,-11.4283172433782,10.6950739523901));
#15179=CARTESIAN_POINT('Ctrl Pts',(15.3208543776412,-11.9195411796877,10.9279323587878));
#15180=CARTESIAN_POINT('Ctrl Pts',(15.594651876132,-12.2002349513456,11.0610183419671));
#15181=CARTESIAN_POINT('Ctrl Pts',(15.7315506253773,-12.3405832861097,11.1275551370522));
#15182=CARTESIAN_POINT('Ctrl Pts',(15.8,-12.4107561622081,11.1608290568883));
#15183=CARTESIAN_POINT('Ctrl Pts',(10.0502525316942,-6.25935291859365,8.32768215464935));
#15184=CARTESIAN_POINT('Ctrl Pts',(11.1454425256572,-7.35179456409855,8.87221159590508));
#15185=CARTESIAN_POINT('Ctrl Pts',(12.3775312688656,-8.58070593097969,9.48507728715608));
#15186=CARTESIAN_POINT('Ctrl Pts',(13.7465187613193,-9.94625006691877,10.1657641132886));
#15187=CARTESIAN_POINT('Ctrl Pts',(14.2941137583008,-10.4924666723322,10.4380421577189));
#15188=CARTESIAN_POINT('Ctrl Pts',(14.8417087552823,-11.0386735802612,10.7103508393265));
#15189=CARTESIAN_POINT('Ctrl Pts',(15.3208543776411,-11.5166076371098,10.9486114186505));
#15190=CARTESIAN_POINT('Ctrl Pts',(15.5946518761319,-11.7897165434404,11.0847485338421));
#15191=CARTESIAN_POINT('Ctrl Pts',(15.7315506253773,-11.9262700347798,11.1528201301259));
#15192=CARTESIAN_POINT('Ctrl Pts',(15.8,-11.9945476376238,11.1868532202043));
#15193=CARTESIAN_POINT('Ctrl Pts',(10.0502525316942,-6.10559301495173,8.23761851725689));
#15194=CARTESIAN_POINT('Ctrl Pts',(11.1454425256572,-7.17588579216885,8.78181727442991));
#15195=CARTESIAN_POINT('Ctrl Pts',(12.3775312688656,-8.37997276877534,9.39427431712614));
#15196=CARTESIAN_POINT('Ctrl Pts',(13.7465187613193,-9.71783944471699,10.0745443941304));
#15197=CARTESIAN_POINT('Ctrl Pts',(14.2941137583009,-10.2529862083793,10.3466552894421));
#15198=CARTESIAN_POINT('Ctrl Pts',(14.8417087552824,-10.7881338344522,10.61879266668));
#15199=CARTESIAN_POINT('Ctrl Pts',(15.3208543776412,-11.2563877393682,10.856904645461));
#15200=CARTESIAN_POINT('Ctrl Pts',(15.5946518761319,-11.5239610675182,10.9929584447386));
#15201=CARTESIAN_POINT('Ctrl Pts',(15.7315506253773,-11.6577478171298,11.060987970935));
#15202=CARTESIAN_POINT('Ctrl Pts',(15.8,-11.7246411157058,11.0950003932583));
#15203=CARTESIAN_POINT('Ctrl Pts',(10.0502525316942,-5.94621492062453,8.15474945546092));
#15204=CARTESIAN_POINT('Ctrl Pts',(11.1454425256572,-6.99511596848632,8.69826758958589));
#15205=CARTESIAN_POINT('Ctrl Pts',(12.3775312688656,-8.17501015002259,9.30992859260386));
#15206=CARTESIAN_POINT('Ctrl Pts',(13.7465187613193,-9.48612538727718,9.98934507962172));
#15207=CARTESIAN_POINT('Ctrl Pts',(14.2941137583008,-10.0105700158496,10.2611141666576));
#15208=CARTESIAN_POINT('Ctrl Pts',(14.8417087552823,-10.535001088446,10.532906293941));
#15209=CARTESIAN_POINT('Ctrl Pts',(15.3208543776412,-10.9938824879741,10.7707172481292));
#15210=CARTESIAN_POINT('Ctrl Pts',(15.5946518761319,-11.2561056460575,10.9066003574976));
#15211=CARTESIAN_POINT('Ctrl Pts',(15.7315506253773,-11.3872158805765,10.9745441973833));
#15212=CARTESIAN_POINT('Ctrl Pts',(15.8,-11.4527721960679,11.0085140807661));
#15213=CARTESIAN_POINT('Ctrl Pts',(10.0502525316942,-5.69326714724858,8.04752551167497));
#15214=CARTESIAN_POINT('Ctrl Pts',(11.1454425256572,-6.70961935691121,8.59278030111935));
#15215=CARTESIAN_POINT('Ctrl Pts',(12.3775312688656,-7.85307681747465,9.20628631668585));
#15216=CARTESIAN_POINT('Ctrl Pts',(13.7465187613193,-9.12352275260843,9.8878635484672));
#15217=CARTESIAN_POINT('Ctrl Pts',(14.2941137583008,-9.63170187793887,10.1604955992679));
#15218=CARTESIAN_POINT('Ctrl Pts',(14.8417087552824,-10.1398879487016,10.4331383564046));
#15219=CARTESIAN_POINT('Ctrl Pts',(15.3208543776412,-10.5845486031013,10.6716974431005));
#15220=CARTESIAN_POINT('Ctrl Pts',(15.5946518761319,-10.8386377334453,10.8080128020807));
#15221=CARTESIAN_POINT('Ctrl Pts',(15.7315506253773,-10.9656829874862,10.8761715434576));
#15222=CARTESIAN_POINT('Ctrl Pts',(15.8,-11.0292050005901,10.9102499677978));
#15223=CARTESIAN_POINT('Ctrl Pts',(10.0502525316942,-5.49454791241253,7.88548479029562));
#15224=CARTESIAN_POINT('Ctrl Pts',(11.1454425256572,-6.48004349322277,8.42454600598801));
#15225=CARTESIAN_POINT('Ctrl Pts',(12.3775312688655,-7.58873003819356,9.03106484753224));
#15226=CARTESIAN_POINT('Ctrl Pts',(13.7465187613193,-8.82059988637913,9.70489831419833));
#15227=CARTESIAN_POINT('Ctrl Pts',(14.2941137583008,-9.31334787493982,9.97443262085556));
#15228=CARTESIAN_POINT('Ctrl Pts',(14.8417087552823,-9.80609631914575,10.2439754326772));
#15229=CARTESIAN_POINT('Ctrl Pts',(15.3208543776411,-10.237251066285,10.4798227509908));
#15230=CARTESIAN_POINT('Ctrl Pts',(15.5946518761319,-10.4836250322036,10.614589374912));
#15231=CARTESIAN_POINT('Ctrl Pts',(15.7315506253773,-10.6068120603551,10.6819735304405));
#15232=CARTESIAN_POINT('Ctrl Pts',(15.8,-10.6684055341557,10.7156648564213));
#15233=CARTESIAN_POINT('Ctrl Pts',(10.0502525316942,-5.32519947010611,7.70626127860213));
#15234=CARTESIAN_POINT('Ctrl Pts',(11.1454425256572,-6.28278149366022,8.23464403472029));
#15235=CARTESIAN_POINT('Ctrl Pts',(12.3775312688656,-7.36002740501521,8.82914182271552));
#15236=CARTESIAN_POINT('Ctrl Pts',(13.7465187613194,-8.55700179652725,9.48962649341726));
#15237=CARTESIAN_POINT('Ctrl Pts',(14.2941137583009,-9.03579113757913,9.7538211861417));
#15238=CARTESIAN_POINT('Ctrl Pts',(14.8417087552824,-9.5145766369121,10.0180235007137));
#15239=CARTESIAN_POINT('Ctrl Pts',(15.3208543776412,-9.93351514221373,10.2491981583259));
#15240=CARTESIAN_POINT('Ctrl Pts',(15.594651876132,-10.172910051869,10.3812950302632));
#15241=CARTESIAN_POINT('Ctrl Pts',(15.7315506253773,-10.2926071256634,10.4473442221897));
#15242=CARTESIAN_POINT('Ctrl Pts',(15.8,-10.3524560021355,10.4803681444471));
#15243=CARTESIAN_POINT('Ctrl Pts',(10.0502525316942,-5.25663803961482,7.60403044672135));
#15244=CARTESIAN_POINT('Ctrl Pts',(11.1454425256572,-6.20120028598869,8.12499465989843));
#15245=CARTESIAN_POINT('Ctrl Pts',(12.3775312688656,-7.26393484617381,8.71111815506916));
#15246=CARTESIAN_POINT('Ctrl Pts',(13.7465187613193,-8.44464710847935,9.36232701259537));
#15247=CARTESIAN_POINT('Ctrl Pts',(14.2941137583009,-8.91693326542987,9.62281103116557));
#15248=CARTESIAN_POINT('Ctrl Pts',(14.8417087552824,-9.38923099717744,9.88329944620756));
#15249=CARTESIAN_POINT('Ctrl Pts',(15.3208543776412,-9.80248791688055,10.1112254436565));
#15250=CARTESIAN_POINT('Ctrl Pts',(15.5946518761319,-10.0386302748779,10.2414671792814));
#15251=CARTESIAN_POINT('Ctrl Pts',(15.7315506253773,-10.1567026019,10.3065884831493));
#15252=CARTESIAN_POINT('Ctrl Pts',(15.8,-10.2157377422983,10.3391487464728));
#15253=CARTESIAN_POINT('Ctrl Pts',(10.0502525316942,-5.21733945232202,7.53128682236137));
#15254=CARTESIAN_POINT('Ctrl Pts',(11.1454425256572,-6.15376086042613,8.04642571042556));
#15255=CARTESIAN_POINT('Ctrl Pts',(12.3775312688656,-7.20723494454326,8.62595695949777));
#15256=CARTESIAN_POINT('Ctrl Pts',(13.7465187613193,-8.3777617046734,9.269880569578));
#15257=CARTESIAN_POINT('Ctrl Pts',(14.2941137583009,-8.84597240872545,9.52745001361009));
#15258=CARTESIAN_POINT('Ctrl Pts',(14.8417087552824,-9.31418311277751,9.78501945764219));
#15259=CARTESIAN_POINT('Ctrl Pts',(15.3208543776412,-9.72386747882306,10.0103927211703));
#15260=CARTESIAN_POINT('Ctrl Pts',(15.5946518761319,-9.95797283084909,10.1391774431863));
#15261=CARTESIAN_POINT('Ctrl Pts',(15.7315506253773,-10.0750255068621,10.2035698041943));
#15262=CARTESIAN_POINT('Ctrl Pts',(15.8,-10.1335518448686,10.2357659846983));
#15263=CARTESIAN_POINT('Ctrl Pts',(15.8,-10.160938779711,10.2694450138623));
#15264=CARTESIAN_POINT('Ctrl Pts',(15.8,-10.1553950350833,10.2627800357942));
#15265=CARTESIAN_POINT('Ctrl Pts',(15.8,-10.1498844772774,10.2560796357392));
#15266=CARTESIAN_POINT('Ctrl Pts',(15.8,-10.1444070962816,10.2493438236809));
#15267=CARTESIAN_POINT('Ctrl Pts',(15.8,-10.1389628855307,10.242572606579));
#15268=CARTESIAN_POINT('Ctrl Pts',(15.8,-10.1335518448686,10.2357659846983));
#15269=CARTESIAN_POINT('Origin',(15.8,-11.5149238208745,9.70545143020505));
#15270=CARTESIAN_POINT('Ctrl Pts',(10.0502525316942,-4.29750123086779,9.86553218952113));
#15271=CARTESIAN_POINT('Ctrl Pts',(11.9668350211294,-5.98055897313701,11.2772850923971));
#15272=CARTESIAN_POINT('Ctrl Pts',(13.8834175105647,-7.66361671540623,12.689037995273));
#15273=CARTESIAN_POINT('Ctrl Pts',(15.8,-9.34667445767544,14.1007908981489));
#15274=CARTESIAN_POINT('Ctrl Pts',(10.0502525316942,-4.02946472694721,9.92430165934405));
#15275=CARTESIAN_POINT('Ctrl Pts',(11.9668350211294,-5.67542688932036,11.3702854403574));
#15276=CARTESIAN_POINT('Ctrl Pts',(13.8834175105647,-7.32120731702057,12.8166324188796));
#15277=CARTESIAN_POINT('Ctrl Pts',(15.8,-8.96716947939372,14.262616199893));
#15278=CARTESIAN_POINT('Ctrl Pts',(10.0502525316942,-3.61211062987325,9.97045860619055));
#15279=CARTESIAN_POINT('Ctrl Pts',(11.9668350211294,-5.19299729643612,11.4635526451079));
#15280=CARTESIAN_POINT('Ctrl Pts',(13.8834175105647,-6.7741160599007,12.956112555571));
#15281=CARTESIAN_POINT('Ctrl Pts',(15.8,-8.35500272646358,14.4492065944883));
#15282=CARTESIAN_POINT('Ctrl Pts',(10.0502525316942,-3.40259706500424,9.86609404202409));
#15283=CARTESIAN_POINT('Ctrl Pts',(11.9668350211294,-4.93192196434907,11.3629139742223));
#15284=CARTESIAN_POINT('Ctrl Pts',(13.8834175105647,-6.46129704742021,12.8596985741914));
#15285=CARTESIAN_POINT('Ctrl Pts',(15.8,-7.99062194676504,14.3565185063896));
#15286=CARTESIAN_POINT('Ctrl Pts',(10.0502525316942,-3.30601090928165,9.77087387154055));
#15287=CARTESIAN_POINT('Ctrl Pts',(11.9668350211295,-4.80688444200922,11.2600017151873));
#15288=CARTESIAN_POINT('Ctrl Pts',(13.8834175105647,-6.30755492143114,12.7494883087275));
#15289=CARTESIAN_POINT('Ctrl Pts',(15.8,-7.8084284541587,14.2386161523743));
#15290=CARTESIAN_POINT('Ctrl Pts',(10.0502525316942,-3.24522078037662,9.7053049496755));
#15291=CARTESIAN_POINT('Ctrl Pts',(11.9668350211294,-4.72781700580774,11.1883166806211));
#15292=CARTESIAN_POINT('Ctrl Pts',(13.8834175105647,-6.21037804061049,12.6715703878316));
#15293=CARTESIAN_POINT('Ctrl Pts',(15.8,-7.69297426604161,14.1545821187772));
#15294=CARTESIAN_POINT('Ctrl Pts',(10.0502525316942,-3.13558852137588,9.59290229251195));
#15295=CARTESIAN_POINT('Ctrl Pts',(11.9668350211294,-4.58744122478927,11.0646742694966));
#15296=CARTESIAN_POINT('Ctrl Pts',(13.8834175105647,-6.03905717649214,12.5366026187688));
#15297=CARTESIAN_POINT('Ctrl Pts',(15.8,-7.49090987990553,14.0083745957535));
#15298=CARTESIAN_POINT('Ctrl Pts',(10.0502525316942,-2.92757116168118,9.41310152025599));
#15299=CARTESIAN_POINT('Ctrl Pts',(11.9668350211294,-4.32424671627921,10.8702564567215));
#15300=CARTESIAN_POINT('Ctrl Pts',(13.8834175105647,-5.72097159497831,12.3275956094625));
#15301=CARTESIAN_POINT('Ctrl Pts',(15.8,-7.11764714957633,13.784750545928));
#15302=CARTESIAN_POINT('Ctrl Pts',(10.0502525316942,-2.78894862571459,9.19740926566326));
#15303=CARTESIAN_POINT('Ctrl Pts',(11.9668350211294,-4.13765656795514,10.6275127538178));
#15304=CARTESIAN_POINT('Ctrl Pts',(13.8834175105647,-5.48632659127462,12.0577280234798));
#15305=CARTESIAN_POINT('Ctrl Pts',(15.8,-6.83503453351517,13.4878315116343));
#15306=CARTESIAN_POINT('Ctrl Pts',(10.0502525316942,-2.6831512960299,8.97469639188219));
#15307=CARTESIAN_POINT('Ctrl Pts',(11.9668350211294,-3.99115284441713,10.3719655284903));
#15308=CARTESIAN_POINT('Ctrl Pts',(13.8834175105648,-5.29909475352164,11.7692966119437));
#15309=CARTESIAN_POINT('Ctrl Pts',(15.8,-6.60709630190888,13.1665657485518));
#15310=CARTESIAN_POINT('Ctrl Pts',(10.0502525316942,-2.64958522759923,8.85625319397989));
#15311=CARTESIAN_POINT('Ctrl Pts',(11.9668350211294,-3.93994688562079,10.2341088589535));
#15312=CARTESIAN_POINT('Ctrl Pts',(13.8834175105647,-5.23040962052304,11.612095695752));
#15313=CARTESIAN_POINT('Ctrl Pts',(15.8,-6.5207712785446,12.9899513607256));
#15314=CARTESIAN_POINT('Ctrl Pts',(10.0502525316942,-2.63468906623289,8.77492596468499));
#15315=CARTESIAN_POINT('Ctrl Pts',(11.9668350211294,-3.91464433600868,10.1386945339445));
#15316=CARTESIAN_POINT('Ctrl Pts',(13.8834175105647,-5.19459960578447,11.5024631032041));
#15317=CARTESIAN_POINT('Ctrl Pts',(15.8,-6.47455487556026,12.8662316724636));
#15318=CARTESIAN_POINT('Ctrl Pts',(15.8,-6.49019400603777,12.9067253609027));
#15319=CARTESIAN_POINT('Ctrl Pts',(15.8,-6.48698118307512,12.8986734787776));
#15320=CARTESIAN_POINT('Ctrl Pts',(15.8,-6.48381086865141,12.890598163633));
#15321=CARTESIAN_POINT('Ctrl Pts',(15.8,-6.48068305016014,12.8824994218701));
#15322=CARTESIAN_POINT('Ctrl Pts',(15.8,-6.47759771920651,12.874377258079));
#15323=CARTESIAN_POINT('Ctrl Pts',(15.8,-6.47455487556026,12.8662316724636));
#15324=CARTESIAN_POINT('Origin',(15.8,-7.95219390447097,12.7887399758658));
#15325=CARTESIAN_POINT('Ctrl Pts',(10.0502525316942,-1.03854944428814,10.7106795892491));
#15326=CARTESIAN_POINT('Ctrl Pts',(11.9668350211294,-2.20297683852746,12.5734298318033));
#15327=CARTESIAN_POINT('Ctrl Pts',(13.8834175105647,-3.36740423276678,14.4361800743576));
#15328=CARTESIAN_POINT('Ctrl Pts',(15.8,-4.5318316270061,16.2989303169119));
#15329=CARTESIAN_POINT('Ctrl Pts',(10.0502525316942,-0.765470815703814,
10.6837448416591));
#15330=CARTESIAN_POINT('Ctrl Pts',(11.9668350211294,-1.88404029388038,12.5675874193204));
#15331=CARTESIAN_POINT('Ctrl Pts',(13.8834175105647,-3.00232469790949,14.4517192592367));
#15332=CARTESIAN_POINT('Ctrl Pts',(15.8,-4.12089417608606,16.335561836898));
#15333=CARTESIAN_POINT('Ctrl Pts',(10.0502525316942,-0.354275884655605,
10.5986742216641));
#15334=CARTESIAN_POINT('Ctrl Pts',(11.9668350211295,-1.39639701818897,12.5072118829665));
#15335=CARTESIAN_POINT('Ctrl Pts',(13.8834175105647,-2.43890221878171,14.4153151096237));
#15336=CARTESIAN_POINT('Ctrl Pts',(15.8,-3.48102335231507,16.3238527709261));
#15337=CARTESIAN_POINT('Ctrl Pts',(10.0502525316942,-0.187261072828498,
10.4346757823309));
#15338=CARTESIAN_POINT('Ctrl Pts',(11.9668350211295,-1.17919268731443,12.3308235163868));
#15339=CARTESIAN_POINT('Ctrl Pts',(13.8834175105647,-2.17117887432507,14.2269575174279));
#15340=CARTESIAN_POINT('Ctrl Pts',(15.8,-3.163110488811,16.1231052514838));
#15341=CARTESIAN_POINT('Ctrl Pts',(10.0502525316942,-0.124824203483033,
10.3142698682631));
#15342=CARTESIAN_POINT('Ctrl Pts',(11.9668350211295,-1.09207394643473,12.1943100355803));
#15343=CARTESIAN_POINT('Ctrl Pts',(13.8834175105647,-2.05901454824882,14.0746341437949));
#15344=CARTESIAN_POINT('Ctrl Pts',(15.8,-3.02626429120052,15.9546743111122));
#15345=CARTESIAN_POINT('Ctrl Pts',(10.0502525316942,-0.0872711810328558,
10.2331249635989));
#15346=CARTESIAN_POINT('Ctrl Pts',(11.9668350211295,-1.03902815454411,12.1017003635113));
#15347=CARTESIAN_POINT('Ctrl Pts',(13.8834175105647,-1.99067177195528,13.9705005205662));
#15348=CARTESIAN_POINT('Ctrl Pts',(15.8,-2.94242874546654,15.8390759204785));
#15349=CARTESIAN_POINT('Ctrl Pts',(10.0502525316942,-0.0177390798696548,
10.09234540735));
#15350=CARTESIAN_POINT('Ctrl Pts',(11.9668350211294,-0.943730501418606,
11.9407308952458));
#15351=CARTESIAN_POINT('Ctrl Pts',(13.8834175105647,-1.86944300220408,13.789197555515));
#15352=CARTESIAN_POINT('Ctrl Pts',(15.8,-2.79543442375304,15.6375830434108));
#15353=CARTESIAN_POINT('Ctrl Pts',(10.0502525316942,0.124535428292433,9.85706386916291));
#15354=CARTESIAN_POINT('Ctrl Pts',(11.9668350211295,-0.753496320252986,
11.6744970487389));
#15355=CARTESIAN_POINT('Ctrl Pts',(13.8834175105647,-1.63151416409049,13.4921256030567));
#15356=CARTESIAN_POINT('Ctrl Pts',(15.8,-2.50954591263591,15.3095587826327));
#15357=CARTESIAN_POINT('Ctrl Pts',(10.0502525316942,0.189717758784555,9.60909091476054));
#15358=CARTESIAN_POINT('Ctrl Pts',(11.9668350211294,-0.651053436707715,
11.3859738307471));
#15359=CARTESIAN_POINT('Ctrl Pts',(13.8834175105647,-1.49175101418763,13.1629551482145));
#15360=CARTESIAN_POINT('Ctrl Pts',(15.8,-2.3325222096799,14.9398380642011));
#15361=CARTESIAN_POINT('Ctrl Pts',(10.0502525316942,0.221513186022213,9.36458479377687));
#15362=CARTESIAN_POINT('Ctrl Pts',(11.9668350211294,-0.590690300968109,
11.0976614182865));
#15363=CARTESIAN_POINT('Ctrl Pts',(13.8834175105648,-1.40281548080796,12.8307816497324));
#15364=CARTESIAN_POINT('Ctrl Pts',(15.8,-2.21501896779828,14.563858274242));
#15365=CARTESIAN_POINT('Ctrl Pts',(10.0502525316942,0.21682744723956,9.24156417346731));
#15366=CARTESIAN_POINT('Ctrl Pts',(11.9668350211294,-0.58459859972662,10.9507264633732));
#15367=CARTESIAN_POINT('Ctrl Pts',(13.8834175105647,-1.38608024219576,12.6600447395717));
#15368=CARTESIAN_POINT('Ctrl Pts',(15.8,-2.18750628916194,14.3692070294775));
#15369=CARTESIAN_POINT('Ctrl Pts',(10.0502525316942,0.205863042617261,9.15961421508102));
#15370=CARTESIAN_POINT('Ctrl Pts',(11.9668350211294,-0.590019092973717,
10.8521631299943));
#15371=CARTESIAN_POINT('Ctrl Pts',(13.8834175105647,-1.38590122856469,12.5447120449076));
#15372=CARTESIAN_POINT('Ctrl Pts',(15.8,-2.18178336415567,14.2372609598209));
#15373=CARTESIAN_POINT('Ctrl Pts',(15.8,-2.18414382321291,14.2806055031745));
#15374=CARTESIAN_POINT('Ctrl Pts',(15.8,-2.18357641541193,14.2719548913156));
#15375=CARTESIAN_POINT('Ctrl Pts',(15.8,-2.18305667683518,14.2632951291918));
#15376=CARTESIAN_POINT('Ctrl Pts',(15.8,-2.18258459351507,14.2546262189952));
#15377=CARTESIAN_POINT('Ctrl Pts',(15.8,-2.18216015604922,14.2459481624974));
#15378=CARTESIAN_POINT('Ctrl Pts',(15.8,-2.18178336415567,14.2372609598209));
#15379=CARTESIAN_POINT('Origin',(15.8,-3.61104784250494,14.6201775482978));
#15380=CARTESIAN_POINT('Ctrl Pts',(10.0502525316942,2.32206279789789,10.5073910450885));
#15381=CARTESIAN_POINT('Ctrl Pts',(11.1454425256572,2.01816863800157,11.7253388222013));
#15382=CARTESIAN_POINT('Ctrl Pts',(12.3775312688656,1.67628770811821,13.0955300714531));
#15383=CARTESIAN_POINT('Ctrl Pts',(13.7465187613194,1.29642000824781,14.617964792844));
#15384=CARTESIAN_POINT('Ctrl Pts',(14.2941137583009,1.14447292829964,15.2269386814004));
#15385=CARTESIAN_POINT('Ctrl Pts',(14.8417087552824,0.992525848351482,15.8359125699568));
#15386=CARTESIAN_POINT('Ctrl Pts',(15.3208543776412,0.859572153396841,16.3687647224436));
#15387=CARTESIAN_POINT('Ctrl Pts',(15.5946518761319,0.78359861342276,16.6732516667218));
#15388=CARTESIAN_POINT('Ctrl Pts',(15.7315506253773,0.74561184343572,16.8254951388609));
#15389=CARTESIAN_POINT('Ctrl Pts',(15.8,0.7266184584422,16.9016168749304));
#15390=CARTESIAN_POINT('Ctrl Pts',(10.0502525316942,2.57345271232945,10.3973886408451));
#15391=CARTESIAN_POINT('Ctrl Pts',(11.1454425256572,2.29815463811993,11.618687280661));
#15392=CARTESIAN_POINT('Ctrl Pts',(12.3775312688656,1.98887116228557,12.9928273987101));
#15393=CARTESIAN_POINT('Ctrl Pts',(13.7465187613193,1.64478997784957,14.519468077176));
#15394=CARTESIAN_POINT('Ctrl Pts',(14.2941137583009,1.50716238874916,15.1301263986154));
#15395=CARTESIAN_POINT('Ctrl Pts',(14.8417087552824,1.36958497392712,15.740805777741));
#15396=CARTESIAN_POINT('Ctrl Pts',(15.3208543776412,1.24918922664557,16.2751437253593));
#15397=CARTESIAN_POINT('Ctrl Pts',(15.5946518761319,1.18037249165619,16.5804716520035));
#15398=CARTESIAN_POINT('Ctrl Pts',(15.7315506253773,1.14596909077302,16.7331376997671));
#15399=CARTESIAN_POINT('Ctrl Pts',(15.8,1.12876296113493,16.8094688647556));
#15400=CARTESIAN_POINT('Ctrl Pts',(10.0502525316942,2.93870070814822,10.1893681184011));
#15401=CARTESIAN_POINT('Ctrl Pts',(11.1454425256572,2.70946206711307,11.4106316171747));
#15402=CARTESIAN_POINT('Ctrl Pts',(12.3775312688656,2.45105312324518,12.7843360022416));
#15403=CARTESIAN_POINT('Ctrl Pts',(13.7465187613194,2.16445481731472,14.310894320163));
#15404=CARTESIAN_POINT('Ctrl Pts',(14.2941137583009,2.04980959621706,14.9215151635443));
#15405=CARTESIAN_POINT('Ctrl Pts',(14.8417087552824,1.93510378473095,15.5321104940175));
#15406=CARTESIAN_POINT('Ctrl Pts',(15.3208543776412,1.83475492870442,16.0663892944466));
#15407=CARTESIAN_POINT('Ctrl Pts',(15.5946518761319,1.77743586902583,16.3717012113088));
#15408=CARTESIAN_POINT('Ctrl Pts',(15.7315506253773,1.74877034151339,16.5243546442885));
#15409=CARTESIAN_POINT('Ctrl Pts',(15.8,1.7344429264487,16.6006836129618));
#15410=CARTESIAN_POINT('Ctrl Pts',(10.0502525316942,3.05808383535425,9.95881139224216));
#15411=CARTESIAN_POINT('Ctrl Pts',(11.1454425256572,2.85649631904974,11.1626816238277));
#15412=CARTESIAN_POINT('Ctrl Pts',(12.3775312688655,2.62997738853437,12.5171248305866));
#15413=CARTESIAN_POINT('Ctrl Pts',(13.7465187613193,2.37801889657081,14.0219712727572));
#15414=CARTESIAN_POINT('Ctrl Pts',(14.2941137583008,2.27723855544496,14.6239108703275));
#15415=CARTESIAN_POINT('Ctrl Pts',(14.8417087552823,2.17648960137064,15.225860952321));
#15416=CARTESIAN_POINT('Ctrl Pts',(15.3208543776411,2.08832456454097,15.7525640332375));
#15417=CARTESIAN_POINT('Ctrl Pts',(15.5946518761319,2.03793255455516,16.0535332175881));
#15418=CARTESIAN_POINT('Ctrl Pts',(15.7315506253773,2.01273965647872,16.2040188475872));
#15419=CARTESIAN_POINT('Ctrl Pts',(15.7999999999999,2.00014043670969,16.2792607370613));
#15420=CARTESIAN_POINT('Ctrl Pts',(10.0502525316942,3.07559947603193,9.78147886731911));
#15421=CARTESIAN_POINT('Ctrl Pts',(11.1454425256572,2.88676320881926,10.9672359168267));
#15422=CARTESIAN_POINT('Ctrl Pts',(12.3775312688655,2.67450622091511,12.3013551830101));
#15423=CARTESIAN_POINT('Ctrl Pts',(13.7465187613193,2.43847871808159,13.7835653267336));
#15424=CARTESIAN_POINT('Ctrl Pts',(14.2941137583008,2.34406982037812,14.3764510158762));
#15425=CARTESIAN_POINT('Ctrl Pts',(14.8417087552823,2.24968252863639,14.9693534649946));
#15426=CARTESIAN_POINT('Ctrl Pts',(15.3208543776412,2.16708696976892,15.4881379273167));
#15427=CARTESIAN_POINT('Ctrl Pts',(15.5946518761319,2.11988125471031,15.7845797896778));
#15428=CARTESIAN_POINT('Ctrl Pts',(15.7315506253773,2.09628053589475,15.9328023798814));
#15429=CARTESIAN_POINT('Ctrl Pts',(15.8,2.08447826919396,16.0069121954756));
#15430=CARTESIAN_POINT('Ctrl Pts',(10.0502525316941,3.10223684531879,9.60383008034198));
#15431=CARTESIAN_POINT('Ctrl Pts',(11.1454425256572,2.92542368552957,10.771880797072));
#15432=CARTESIAN_POINT('Ctrl Pts',(12.3775312688655,2.72674232124833,12.0859609655105));
#15433=CARTESIAN_POINT('Ctrl Pts',(13.7465187613193,2.5057485169523,13.5460266034681));
#15434=CARTESIAN_POINT('Ctrl Pts',(14.2941137583008,2.41735366657091,14.1300531231308));
#15435=CARTESIAN_POINT('Ctrl Pts',(14.8417087552823,2.32898625556579,14.7140823594691));
#15436=CARTESIAN_POINT('Ctrl Pts',(15.3208543776411,2.25165628918294,15.2251071015168));
#15437=CARTESIAN_POINT('Ctrl Pts',(15.5946518761319,2.20745725592094,15.5171202021387));
#15438=CARTESIAN_POINT('Ctrl Pts',(15.7315506253773,2.18536045543708,15.6631270213657));
#15439=CARTESIAN_POINT('Ctrl Pts',(15.8,2.17430963295026,15.7361301911614));
#15440=CARTESIAN_POINT('Ctrl Pts',(10.0502525316942,3.1641697547985,9.33616641898041));
#15441=CARTESIAN_POINT('Ctrl Pts',(11.1454425256572,3.00789330574878,10.4789053528453));
#15442=CARTESIAN_POINT('Ctrl Pts',(12.3775312688656,2.83212323706008,11.7645911992084));
#15443=CARTESIAN_POINT('Ctrl Pts',(13.7465187613193,2.6367816468882,13.1930250082462));
#15444=CARTESIAN_POINT('Ctrl Pts',(14.2941137583008,2.55864547926934,13.7643997282132));
#15445=CARTESIAN_POINT('Ctrl Pts',(14.8417087552823,2.48051412346292,14.3357867368397));
#15446=CARTESIAN_POINT('Ctrl Pts',(15.3208543776412,2.4121476997586,14.8357465708549));
#15447=CARTESIAN_POINT('Ctrl Pts',(15.5946518761319,2.37307933395524,15.1214332106675));
#15448=CARTESIAN_POINT('Ctrl Pts',(15.7315506253773,2.35354562736143,15.2642777469938));
#15449=CARTESIAN_POINT('Ctrl Pts',(15.8,2.34377834929582,15.3356989303604));
#15450=CARTESIAN_POINT('Ctrl Pts',(10.0502525316942,3.14987939962279,9.08015411140619));
#15451=CARTESIAN_POINT('Ctrl Pts',(11.1454425256572,3.00672931552669,10.1942890168299));
#15452=CARTESIAN_POINT('Ctrl Pts',(12.3775312688655,2.84574388114627,11.4477380681646));
#15453=CARTESIAN_POINT('Ctrl Pts',(13.7465187613193,2.66681194224705,12.8404112867165));
#15454=CARTESIAN_POINT('Ctrl Pts',(14.2941137583008,2.59523983509501,13.3974811152093));
#15455=CARTESIAN_POINT('Ctrl Pts',(14.8417087552823,2.52367459367682,13.9545565014729));
#15456=CARTESIAN_POINT('Ctrl Pts',(15.3208543776411,2.46105288517697,14.4419957464976));
#15457=CARTESIAN_POINT('Ctrl Pts',(15.5946518761319,2.42526642923796,14.7205303350335));
#15458=CARTESIAN_POINT('Ctrl Pts',(15.7315506253773,2.40737388088825,14.8597981794497));
#15459=CARTESIAN_POINT('Ctrl Pts',(15.8,2.39842700063224,14.9294316110387));
#15460=CARTESIAN_POINT('Ctrl Pts',(10.0502525316942,3.10442465522081,8.83780343943476));
#15461=CARTESIAN_POINT('Ctrl Pts',(11.1454425256572,2.96904269314958,9.92307916160989));
#15462=CARTESIAN_POINT('Ctrl Pts',(12.3775312688656,2.81681208487056,11.1440266947135));
#15463=CARTESIAN_POINT('Ctrl Pts',(13.7465187613194,2.64759182043347,12.5006225450517));
#15464=CARTESIAN_POINT('Ctrl Pts',(14.2941137583009,2.5799045625987,13.0432610264625));
#15465=CARTESIAN_POINT('Ctrl Pts',(14.8417087552824,2.51222601461465,13.585900959023));
#15466=CARTESIAN_POINT('Ctrl Pts',(15.3208543776412,2.45300459283688,14.0607104514503));
#15467=CARTESIAN_POINT('Ctrl Pts',(15.594651876132,2.41916045348293,14.3320296071118));
#15468=CARTESIAN_POINT('Ctrl Pts',(15.7315506253773,2.40223924596973,14.4676893285878));
#15469=CARTESIAN_POINT('Ctrl Pts',(15.8,2.39377787334028,14.5355190612237));
#15470=CARTESIAN_POINT('Ctrl Pts',(10.0502525316942,3.06201554081689,8.72224646189197));
#15471=CARTESIAN_POINT('Ctrl Pts',(11.1454425256572,2.92828468444751,9.79262845293104));
#15472=CARTESIAN_POINT('Ctrl Pts',(12.3775312688656,2.77780914227504,10.9969124481398));
#15473=CARTESIAN_POINT('Ctrl Pts',(13.7465187613194,2.61064282371592,12.3349000504671));
#15474=CARTESIAN_POINT('Ctrl Pts',(14.2941137583009,2.54377597211689,12.870096284426));
#15475=CARTESIAN_POINT('Ctrl Pts',(14.8417087552824,2.47690579066087,13.4053047729009));
#15476=CARTESIAN_POINT('Ctrl Pts',(15.3208543776412,2.41839541117503,13.8736084123374));
#15477=CARTESIAN_POINT('Ctrl Pts',(15.5946518761319,2.38496218052017,14.1412058111469));
#15478=CARTESIAN_POINT('Ctrl Pts',(15.7315506253773,2.3682452355795,14.2750057235919));
#15479=CARTESIAN_POINT('Ctrl Pts',(15.8,2.35988705705641,14.3419045980318));
#15480=CARTESIAN_POINT('Ctrl Pts',(10.0502525316942,3.02626384252387,8.64769560732005));
#15481=CARTESIAN_POINT('Ctrl Pts',(11.1454425256572,2.89260526381666,9.70806748165927));
#15482=CARTESIAN_POINT('Ctrl Pts',(12.3775312688656,2.74223936277106,10.9009858402909));
#15483=CARTESIAN_POINT('Ctrl Pts',(13.7465187613194,2.57516613938705,12.2264506832149));
#15484=CARTESIAN_POINT('Ctrl Pts',(14.2941137583009,2.50833685003344,12.7566366203845));
#15485=CARTESIAN_POINT('Ctrl Pts',(14.8417087552824,2.44150756067984,13.2868225575541));
#15486=CARTESIAN_POINT('Ctrl Pts',(15.3208543776412,2.38303193249543,13.7507352525775));
#15487=CARTESIAN_POINT('Ctrl Pts',(15.5946518761319,2.34961728781863,14.0158282211623));
#15488=CARTESIAN_POINT('Ctrl Pts',(15.7315506253773,2.33290996548023,14.1483747054547));
#15489=CARTESIAN_POINT('Ctrl Pts',(15.8,2.32455630431103,14.2146479476009));
#15490=CARTESIAN_POINT('Ctrl Pts',(15.8,2.33570557485288,14.2566004799664));
#15491=CARTESIAN_POINT('Ctrl Pts',(15.8,2.33357202566325,14.2481979205348));
#15492=CARTESIAN_POINT('Ctrl Pts',(15.8,2.33139031275994,14.2398013892846));
#15493=CARTESIAN_POINT('Ctrl Pts',(15.8,2.32916045010432,14.2314108839843));
#15494=CARTESIAN_POINT('Ctrl Pts',(15.8,2.32688244718599,14.2230264034132));
#15495=CARTESIAN_POINT('Ctrl Pts',(15.8,2.32455630431103,14.2146479476009));
#15496=CARTESIAN_POINT('Origin',(15.8,1.08357274193521,15.0204902775358));
#15497=CARTESIAN_POINT('Ctrl Pts',(10.0502525316942,5.45537535466284,9.2755658561365));
#15498=CARTESIAN_POINT('Ctrl Pts',(11.1454425256572,5.54272139501843,10.527811485966));
#15499=CARTESIAN_POINT('Ctrl Pts',(12.3775312688656,5.64098569041847,11.9365878195243));
#15500=CARTESIAN_POINT('Ctrl Pts',(13.7465187613193,5.75016824086295,13.5018948568112));
#15501=CARTESIAN_POINT('Ctrl Pts',(14.2941137583009,5.79384126104075,14.1280176717259));
#15502=CARTESIAN_POINT('Ctrl Pts',(14.8417087552824,5.83751428121855,14.7541404866407));
#15503=CARTESIAN_POINT('Ctrl Pts',(15.3208543776412,5.87572817387412,15.3019979496911));
#15504=CARTESIAN_POINT('Ctrl Pts',(15.5946518761319,5.89756468396301,15.6150593571485));
#15505=CARTESIAN_POINT('Ctrl Pts',(15.7315506253773,5.90848293900746,15.7715900608772));
#15506=CARTESIAN_POINT('Ctrl Pts',(15.8,5.91394206652969,15.8498554127416));
#15507=CARTESIAN_POINT('Ctrl Pts',(10.0502525316942,5.66046875858054,9.09326359699885));
#15508=CARTESIAN_POINT('Ctrl Pts',(11.1454425256572,5.77604676609019,10.3398594101876));
#15509=CARTESIAN_POINT('Ctrl Pts',(12.3775312688656,5.90654052031257,11.7423187718539));
#15510=CARTESIAN_POINT('Ctrl Pts',(13.7465187613193,6.05105541408884,13.3005670731329));
#15511=CARTESIAN_POINT('Ctrl Pts',(14.2941137583009,6.10886731837784,13.9238668895967));
#15512=CARTESIAN_POINT('Ctrl Pts',(14.8417087552824,6.16673138983644,14.5471710567224));
#15513=CARTESIAN_POINT('Ctrl Pts',(15.3208543776412,6.2173462055988,15.0925608480022));
#15514=CARTESIAN_POINT('Ctrl Pts',(15.5946518761319,6.24624880770451,15.404210476846));
#15515=CARTESIAN_POINT('Ctrl Pts',(15.7315506253773,6.26070528969668,15.5600357233503));
#15516=CARTESIAN_POINT('Ctrl Pts',(15.8,6.26792891516603,15.6379479616746));
#15517=CARTESIAN_POINT('Ctrl Pts',(10.0502525316942,5.94355560685308,8.78255765938312));
#15518=CARTESIAN_POINT('Ctrl Pts',(11.1454425256572,6.10292787924083,10.0148869038525));
#15519=CARTESIAN_POINT('Ctrl Pts',(12.3775312688656,6.2816544949474,11.4012092316412));
#15520=CARTESIAN_POINT('Ctrl Pts',(13.7465187613194,6.48081852219945,12.9416164381759));
#15521=CARTESIAN_POINT('Ctrl Pts',(14.2941137583009,6.56047693355264,13.5577787105923));
#15522=CARTESIAN_POINT('Ctrl Pts',(14.8417087552824,6.64007218801815,14.1739356301478));
#15523=CARTESIAN_POINT('Ctrl Pts',(15.3208543776412,6.70973770503939,14.7130746018355));
#15524=CARTESIAN_POINT('Ctrl Pts',(15.5946518761319,6.74957096648566,15.0211560817904));
#15525=CARTESIAN_POINT('Ctrl Pts',(15.7315506253773,6.76948132483472,15.1751962901529));
#15526=CARTESIAN_POINT('Ctrl Pts',(15.8,6.77944209185895,15.2522168679322));
#15527=CARTESIAN_POINT('Ctrl Pts',(10.0502525316942,5.9858465900355,8.52639512605654));
#15528=CARTESIAN_POINT('Ctrl Pts',(11.1454425256572,6.16614182963238,9.73363772297169));
#15529=CARTESIAN_POINT('Ctrl Pts',(12.3775312688656,6.36925721416674,11.0917875706281));
#15530=CARTESIAN_POINT('Ctrl Pts',(13.7465187613193,6.59465188812854,12.6008409910269));
#15531=CARTESIAN_POINT('Ctrl Pts',(14.2941137583008,6.68481335297614,13.2044623836355));
#15532=CARTESIAN_POINT('Ctrl Pts',(14.8417087552823,6.77500635669624,13.8080839907189));
#15533=CARTESIAN_POINT('Ctrl Pts',(15.3208543776411,6.85391541259334,14.3362528301216));
#15534=CARTESIAN_POINT('Ctrl Pts',(15.5946518761319,6.89899411967347,14.6380635126529));
#15535=CARTESIAN_POINT('Ctrl Pts',(15.7315506253773,6.92153660547059,14.7889688752189));
#15536=CARTESIAN_POINT('Ctrl Pts',(15.8,6.93280505794539,14.8644215375261));
#15537=CARTESIAN_POINT('Ctrl Pts',(10.0502525316942,5.94770436886827,8.35233000922534));
#15538=CARTESIAN_POINT('Ctrl Pts',(11.1454425256572,6.13452948592055,9.53840559362551));
#15539=CARTESIAN_POINT('Ctrl Pts',(12.3775312688656,6.34492663085592,10.8728200811769));
#15540=CARTESIAN_POINT('Ctrl Pts',(13.7465187613193,6.57847782979354,12.3554217499083));
#15541=CARTESIAN_POINT('Ctrl Pts',(14.2941137583008,6.67190108779269,12.9484634259519));
#15542=CARTESIAN_POINT('Ctrl Pts',(14.8417087552824,6.76534871907581,13.5415139493489));
#15543=CARTESIAN_POINT('Ctrl Pts',(15.3208543776412,6.84710780571679,14.0604304019321));
#15544=CARTESIAN_POINT('Ctrl Pts',(15.5946518761319,6.89381786952799,14.3569506718));
#15545=CARTESIAN_POINT('Ctrl Pts',(15.7315506253773,6.91717532204614,14.5052116854016));
#15546=CARTESIAN_POINT('Ctrl Pts',(15.8,6.92885189186191,14.5793414094266));
#15547=CARTESIAN_POINT('Ctrl Pts',(10.0502525316942,5.91814205125966,8.17514436986861));
#15548=CARTESIAN_POINT('Ctrl Pts',(11.1454425256572,6.1109302652368,9.34066488658196));
#15549=CARTESIAN_POINT('Ctrl Pts',(12.3775312688656,6.32804641946554,10.6518240329443));
#15550=CARTESIAN_POINT('Ctrl Pts',(13.7465187613193,6.56905244176937,12.1087200255634));
#15551=CARTESIAN_POINT('Ctrl Pts',(14.2941137583008,6.66545776271566,12.6914777697296));
#15552=CARTESIAN_POINT('Ctrl Pts',(14.8417087552823,6.76188862893654,13.2742297865971));
#15553=CARTESIAN_POINT('Ctrl Pts',(15.3208543776412,6.84625768114734,13.7841395850464));
#15554=CARTESIAN_POINT('Ctrl Pts',(15.5946518761319,6.89445870116996,14.0755188249216));
#15555=CARTESIAN_POINT('Ctrl Pts',(15.7315506253773,6.91856174818909,14.2212078760573));
#15556=CARTESIAN_POINT('Ctrl Pts',(15.8,6.93061101156266,14.2940529083519));
#15557=CARTESIAN_POINT('Ctrl Pts',(10.0502525316942,5.89433124999992,7.90144264462466));
#15558=CARTESIAN_POINT('Ctrl Pts',(11.1454425256572,6.09882926548586,9.03654403267793));
#15559=CARTESIAN_POINT('Ctrl Pts',(12.3775312688656,6.32895925304843,10.3136205759384));
#15560=CARTESIAN_POINT('Ctrl Pts',(13.7465187613193,6.58458807992398,11.7325052253954));
#15561=CARTESIAN_POINT('Ctrl Pts',(14.2941137583008,6.68684049565601,12.3000601956136));
#15562=CARTESIAN_POINT('Ctrl Pts',(14.8417087552823,6.7891006747503,12.86762490695));
#15563=CARTESIAN_POINT('Ctrl Pts',(15.3208543776412,6.87857591366295,13.364240995629));
#15564=CARTESIAN_POINT('Ctrl Pts',(15.5946518761319,6.9297016229862,13.648017855189));
#15565=CARTESIAN_POINT('Ctrl Pts',(15.7315506253773,6.95526524865973,13.7899072524002));
#15566=CARTESIAN_POINT('Ctrl Pts',(15.8,6.9680463746276,13.8608510891535));
#15567=CARTESIAN_POINT('Ctrl Pts',(10.0502525316942,5.80163007173556,7.66237562613099));
#15568=CARTESIAN_POINT('Ctrl Pts',(11.1454425256572,6.00977287125003,8.76621669669801));
#15569=CARTESIAN_POINT('Ctrl Pts',(12.3775312688656,6.24400287259233,10.008064757174));
#15570=CARTESIAN_POINT('Ctrl Pts',(13.7465187613193,6.50418764618808,11.3878685250288));
#15571=CARTESIAN_POINT('Ctrl Pts',(14.2941137583008,6.60826243593383,11.9397903730643));
#15572=CARTESIAN_POINT('Ctrl Pts',(14.8417087552823,6.71234494803682,12.4917152115347));
#15573=CARTESIAN_POINT('Ctrl Pts',(15.3208543776411,6.80341474110255,12.9746485138656));
#15574=CARTESIAN_POINT('Ctrl Pts',(15.5946518761319,6.8554516400659,13.2506092458454));
#15575=CARTESIAN_POINT('Ctrl Pts',(15.7315506253773,6.8814708564871,13.3885899088279));
#15576=CARTESIAN_POINT('Ctrl Pts',(15.8,6.89447978145675,13.4575799757384));
#15577=CARTESIAN_POINT('Ctrl Pts',(10.0502525316942,5.68351040711506,7.44593237535689));
#15578=CARTESIAN_POINT('Ctrl Pts',(11.1454425256572,5.89012315163306,8.51992624992032));
#15579=CARTESIAN_POINT('Ctrl Pts',(12.3775312688656,6.12263633930511,9.72815762348206));
#15580=CARTESIAN_POINT('Ctrl Pts',(13.7465187613194,6.38090895110343,11.0706489050024));
#15581=CARTESIAN_POINT('Ctrl Pts',(14.2941137583009,6.48421893322742,11.60764526865));
#15582=CARTESIAN_POINT('Ctrl Pts',(14.8417087552824,6.5875371385849,12.1446403255654));
#15583=CARTESIAN_POINT('Ctrl Pts',(15.3208543776412,6.67793800725713,12.6145114073305));
#15584=CARTESIAN_POINT('Ctrl Pts',(15.594651876132,6.72959247024464,12.8830096730692));
#15585=CARTESIAN_POINT('Ctrl Pts',(15.7315506253773,6.75542051842203,13.0172586761616));
#15586=CARTESIAN_POINT('Ctrl Pts',(15.8,6.7683338149544,13.0843832933218));
#15587=CARTESIAN_POINT('Ctrl Pts',(10.0502525316942,5.60747221894231,7.3491344951621));
#15588=CARTESIAN_POINT('Ctrl Pts',(11.1454425256572,5.81105284226644,8.40845336995524));
#15589=CARTESIAN_POINT('Ctrl Pts',(12.3775312688656,6.04008639989118,9.60029668798143));
#15590=CARTESIAN_POINT('Ctrl Pts',(13.7465187613193,6.29456266363366,10.9244551954278));
#15591=CARTESIAN_POINT('Ctrl Pts',(14.2941137583009,6.3963532371211,11.4541199893924));
#15592=CARTESIAN_POINT('Ctrl Pts',(14.8417087552824,6.49814440704391,11.9837969855611));
#15593=CARTESIAN_POINT('Ctrl Pts',(15.3208543776412,6.58721149497458,12.4472605569962));
#15594=CARTESIAN_POINT('Ctrl Pts',(15.5946518761319,6.63810674341679,12.7120921703849));
#15595=CARTESIAN_POINT('Ctrl Pts',(15.7315506253773,6.66355442687238,12.8445091889311));
#15596=CARTESIAN_POINT('Ctrl Pts',(15.8,6.67627821583013,12.9107166186057));
#15597=CARTESIAN_POINT('Ctrl Pts',(10.0502525316942,5.55043285230422,7.28928030147641));
#15598=CARTESIAN_POINT('Ctrl Pts',(11.1454425256572,5.75098891959401,8.33905665452735));
#15599=CARTESIAN_POINT('Ctrl Pts',(12.3775312688656,5.97661449529503,9.52005505170966));
#15600=CARTESIAN_POINT('Ctrl Pts',(13.7465187613193,6.22730957940727,10.8322754930233));
#15601=CARTESIAN_POINT('Ctrl Pts',(14.2941137583009,6.32758761305217,11.3571636695488));
#15602=CARTESIAN_POINT('Ctrl Pts',(14.8417087552824,6.42786564669707,11.8820518460743));
#15603=CARTESIAN_POINT('Ctrl Pts',(15.3208543776412,6.51560892613635,12.3413290005341));
#15604=CARTESIAN_POINT('Ctrl Pts',(15.5946518761319,6.5657479429588,12.6037730887968));
#15605=CARTESIAN_POINT('Ctrl Pts',(15.7315506253773,6.59081745137003,12.7349951329282));
#15606=CARTESIAN_POINT('Ctrl Pts',(15.8,6.60335220557564,12.8006061549939));
#15607=CARTESIAN_POINT('Ctrl Pts',(15.8,6.62691983743441,12.8370600702028));
#15608=CARTESIAN_POINT('Ctrl Pts',(15.8,6.62229417791417,12.8297280642598));
#15609=CARTESIAN_POINT('Ctrl Pts',(15.8,6.61762457479065,12.8224166748639));
#15610=CARTESIAN_POINT('Ctrl Pts',(15.8,6.61291104065239,12.8151258955788));
#15611=CARTESIAN_POINT('Ctrl Pts',(15.8,6.60815358414732,12.8078557223109));
#15612=CARTESIAN_POINT('Ctrl Pts',(15.8,6.60335220557564,12.8006061549939));
#15613=CARTESIAN_POINT('Origin',(15.8,5.67212567669951,13.950492764499));
#15614=CARTESIAN_POINT('Ctrl Pts',(10.0502525316942,8.05467776187827,7.13578365451838));
#15615=CARTESIAN_POINT('Ctrl Pts',(11.1454425256572,8.52471396348012,8.29974860990865));
#15616=CARTESIAN_POINT('Ctrl Pts',(12.3775312688656,9.05350469028219,9.6092091847227));
#15617=CARTESIAN_POINT('Ctrl Pts',(13.7465187613193,9.6410499422845,11.0641653789605));
#15618=CARTESIAN_POINT('Ctrl Pts',(14.2941137583009,9.87606804308543,11.6461478566557));
#15619=CARTESIAN_POINT('Ctrl Pts',(14.8417087552824,10.1110861438864,12.2281303343508));
#15620=CARTESIAN_POINT('Ctrl Pts',(15.3208543776412,10.3167269820872,12.737365002334));
#15621=CARTESIAN_POINT('Ctrl Pts',(15.5946518761319,10.4342360324876,13.0283562411816));
#15622=CARTESIAN_POINT('Ctrl Pts',(15.7315506253773,10.4929905576879,13.1738518606054));
#15623=CARTESIAN_POINT('Ctrl Pts',(15.8,10.522367820288,13.2465996703173));
#15624=CARTESIAN_POINT('Ctrl Pts',(10.0502525316942,8.19339868393687,6.89902655578542));
#15625=CARTESIAN_POINT('Ctrl Pts',(11.1454425256572,8.68853919251131,8.04889405860839));
#15626=CARTESIAN_POINT('Ctrl Pts',(12.3775312688656,9.24602752966092,9.34238794408147));
#15627=CARTESIAN_POINT('Ctrl Pts',(13.7465187613193,9.86499535005157,10.779712402918));
#15628=CARTESIAN_POINT('Ctrl Pts',(14.2941137583009,10.1125880646808,11.354640872798));
#15629=CARTESIAN_POINT('Ctrl Pts',(14.8417087552824,10.3602324253388,11.9295571981554));
#15630=CARTESIAN_POINT('Ctrl Pts',(15.3208543776412,10.5769051976768,12.4326127553978));
#15631=CARTESIAN_POINT('Ctrl Pts',(15.5946518761319,10.7006983402633,12.7200777462785));
#15632=CARTESIAN_POINT('Ctrl Pts',(15.7315506253773,10.7626000339661,12.8638090371883));
#15633=CARTESIAN_POINT('Ctrl Pts',(15.8,10.793546315752,12.9356757561148));
#15634=CARTESIAN_POINT('Ctrl Pts',(10.0502525316942,8.36661813687799,6.51604789180993));
#15635=CARTESIAN_POINT('Ctrl Pts',(11.1454425256572,8.89900085425541,7.63881390938367));
#15636=CARTESIAN_POINT('Ctrl Pts',(12.3775312688656,9.49738068383038,8.90205445633838));
#15637=CARTESIAN_POINT('Ctrl Pts',(13.7465187613194,10.1628080503653,10.3055239107478));
#15638=CARTESIAN_POINT('Ctrl Pts',(14.2941137583009,10.4289722391039,10.8669132727127));
#15639=CARTESIAN_POINT('Ctrl Pts',(14.8417087552824,10.6950739523901,11.4283172433782));
#15640=CARTESIAN_POINT('Ctrl Pts',(15.3208543776412,10.9279323587878,11.9195411796877));
#15641=CARTESIAN_POINT('Ctrl Pts',(15.594651876132,11.0610183419671,12.2002349513456));
#15642=CARTESIAN_POINT('Ctrl Pts',(15.7315506253773,11.1275551370522,12.3405832861097));
#15643=CARTESIAN_POINT('Ctrl Pts',(15.8,11.1608290568882,12.4107561622081));
#15644=CARTESIAN_POINT('Ctrl Pts',(10.0502525316942,8.32768215464935,6.25935291859365));
#15645=CARTESIAN_POINT('Ctrl Pts',(11.1454425256572,8.87221159590509,7.35179456409855));
#15646=CARTESIAN_POINT('Ctrl Pts',(12.3775312688656,9.48507728715608,8.58070593097969));
#15647=CARTESIAN_POINT('Ctrl Pts',(13.7465187613193,10.1657641132886,9.94625006691877));
#15648=CARTESIAN_POINT('Ctrl Pts',(14.2941137583008,10.4380421577189,10.4924666723322));
#15649=CARTESIAN_POINT('Ctrl Pts',(14.8417087552823,10.7103508393265,11.0386735802612));
#15650=CARTESIAN_POINT('Ctrl Pts',(15.3208543776411,10.9486114186505,11.5166076371098));
#15651=CARTESIAN_POINT('Ctrl Pts',(15.5946518761319,11.0847485338421,11.7897165434404));
#15652=CARTESIAN_POINT('Ctrl Pts',(15.7315506253773,11.1528201301259,11.9262700347798));
#15653=CARTESIAN_POINT('Ctrl Pts',(15.8,11.1868532202043,11.9945476376238));
#15654=CARTESIAN_POINT('Ctrl Pts',(10.0502525316942,8.2376185172569,6.10559301495173));
#15655=CARTESIAN_POINT('Ctrl Pts',(11.1454425256572,8.78181727442992,7.17588579216884));
#15656=CARTESIAN_POINT('Ctrl Pts',(12.3775312688656,9.39427431712613,8.37997276877534));
#15657=CARTESIAN_POINT('Ctrl Pts',(13.7465187613193,10.0745443941304,9.71783944471699));
#15658=CARTESIAN_POINT('Ctrl Pts',(14.2941137583008,10.3466552894421,10.2529862083793));
#15659=CARTESIAN_POINT('Ctrl Pts',(14.8417087552824,10.61879266668,10.7881338344522));
#15660=CARTESIAN_POINT('Ctrl Pts',(15.3208543776412,10.856904645461,11.2563877393682));
#15661=CARTESIAN_POINT('Ctrl Pts',(15.5946518761319,10.9929584447385,11.5239610675182));
#15662=CARTESIAN_POINT('Ctrl Pts',(15.7315506253773,11.0609879709349,11.6577478171298));
#15663=CARTESIAN_POINT('Ctrl Pts',(15.8,11.0950003932583,11.7246411157058));
#15664=CARTESIAN_POINT('Ctrl Pts',(10.0502525316941,8.15474945546093,5.94621492062452));
#15665=CARTESIAN_POINT('Ctrl Pts',(11.1454425256572,8.6982675895859,6.99511596848632));
#15666=CARTESIAN_POINT('Ctrl Pts',(12.3775312688656,9.30992859260386,8.17501015002258));
#15667=CARTESIAN_POINT('Ctrl Pts',(13.7465187613193,9.98934507962172,9.48612538727718));
#15668=CARTESIAN_POINT('Ctrl Pts',(14.2941137583008,10.2611141666576,10.0105700158496));
#15669=CARTESIAN_POINT('Ctrl Pts',(14.8417087552823,10.532906293941,10.535001088446));
#15670=CARTESIAN_POINT('Ctrl Pts',(15.3208543776412,10.7707172481292,10.9938824879741));
#15671=CARTESIAN_POINT('Ctrl Pts',(15.5946518761319,10.9066003574976,11.2561056460575));
#15672=CARTESIAN_POINT('Ctrl Pts',(15.7315506253773,10.9745441973833,11.3872158805765));
#15673=CARTESIAN_POINT('Ctrl Pts',(15.8,11.0085140807661,11.4527721960679));
#15674=CARTESIAN_POINT('Ctrl Pts',(10.0502525316942,8.04752551167497,5.69326714724858));
#15675=CARTESIAN_POINT('Ctrl Pts',(11.1454425256572,8.59278030111936,6.70961935691121));
#15676=CARTESIAN_POINT('Ctrl Pts',(12.3775312688656,9.20628631668581,7.85307681747465));
#15677=CARTESIAN_POINT('Ctrl Pts',(13.7465187613193,9.88786354846716,9.12352275260843));
#15678=CARTESIAN_POINT('Ctrl Pts',(14.2941137583008,10.1604955992679,9.63170187793887));
#15679=CARTESIAN_POINT('Ctrl Pts',(14.8417087552823,10.4331383564046,10.1398879487016));
#15680=CARTESIAN_POINT('Ctrl Pts',(15.3208543776412,10.6716974431005,10.5845486031013));
#15681=CARTESIAN_POINT('Ctrl Pts',(15.5946518761319,10.8080128020806,10.8386377334452));
#15682=CARTESIAN_POINT('Ctrl Pts',(15.7315506253773,10.8761715434575,10.9656829874862));
#15683=CARTESIAN_POINT('Ctrl Pts',(15.8,10.9102499677978,11.0292050005901));
#15684=CARTESIAN_POINT('Ctrl Pts',(10.0502525316942,7.88548479029559,5.49454791241253));
#15685=CARTESIAN_POINT('Ctrl Pts',(11.1454425256572,8.42454600598798,6.48004349322277));
#15686=CARTESIAN_POINT('Ctrl Pts',(12.3775312688655,9.03106484753222,7.58873003819359));
#15687=CARTESIAN_POINT('Ctrl Pts',(13.7465187613193,9.70489831419831,8.82059988637915));
#15688=CARTESIAN_POINT('Ctrl Pts',(14.2941137583008,9.97443262085554,9.31334787493984));
#15689=CARTESIAN_POINT('Ctrl Pts',(14.8417087552823,10.2439754326772,9.80609631914578));
#15690=CARTESIAN_POINT('Ctrl Pts',(15.3208543776411,10.4798227509907,10.2372510662851));
#15691=CARTESIAN_POINT('Ctrl Pts',(15.5946518761319,10.614589374912,10.4836250322036));
#15692=CARTESIAN_POINT('Ctrl Pts',(15.7315506253773,10.6819735304405,10.6068120603551));
#15693=CARTESIAN_POINT('Ctrl Pts',(15.8,10.7156648564213,10.6684055341558));
#15694=CARTESIAN_POINT('Ctrl Pts',(10.0502525316942,7.70626127860213,5.3251994701061));
#15695=CARTESIAN_POINT('Ctrl Pts',(11.1454425256572,8.23464403472029,6.28278149366022));
#15696=CARTESIAN_POINT('Ctrl Pts',(12.3775312688656,8.82914182271548,7.36002740501519));
#15697=CARTESIAN_POINT('Ctrl Pts',(13.7465187613194,9.48962649341722,8.55700179652723));
#15698=CARTESIAN_POINT('Ctrl Pts',(14.2941137583009,9.75382118614165,9.03579113757912));
#15699=CARTESIAN_POINT('Ctrl Pts',(14.8417087552824,10.0180235007136,9.51457663691209));
#15700=CARTESIAN_POINT('Ctrl Pts',(15.3208543776412,10.2491981583259,9.93351514221371));
#15701=CARTESIAN_POINT('Ctrl Pts',(15.594651876132,10.3812950302631,10.172910051869));
#15702=CARTESIAN_POINT('Ctrl Pts',(15.7315506253773,10.4473442221896,10.2926071256633));
#15703=CARTESIAN_POINT('Ctrl Pts',(15.8,10.480368144447,10.3524560021355));
#15704=CARTESIAN_POINT('Ctrl Pts',(10.0502525316942,7.60403044672136,5.25663803961482));
#15705=CARTESIAN_POINT('Ctrl Pts',(11.1454425256572,8.12499465989844,6.2012002859887));
#15706=CARTESIAN_POINT('Ctrl Pts',(12.3775312688656,8.71111815506916,7.26393484617381));
#15707=CARTESIAN_POINT('Ctrl Pts',(13.7465187613193,9.36232701259537,8.44464710847935));
#15708=CARTESIAN_POINT('Ctrl Pts',(14.2941137583009,9.62281103116557,8.91693326542987));
#15709=CARTESIAN_POINT('Ctrl Pts',(14.8417087552824,9.88329944620756,9.38923099717744));
#15710=CARTESIAN_POINT('Ctrl Pts',(15.3208543776412,10.1112254436565,9.80248791688055));
#15711=CARTESIAN_POINT('Ctrl Pts',(15.5946518761319,10.2414671792814,10.0386302748779));
#15712=CARTESIAN_POINT('Ctrl Pts',(15.7315506253773,10.3065884831493,10.1567026019));
#15713=CARTESIAN_POINT('Ctrl Pts',(15.8,10.3391487464728,10.2157377422983));
#15714=CARTESIAN_POINT('Ctrl Pts',(10.0502525316942,7.53128682236137,5.21733945232202));
#15715=CARTESIAN_POINT('Ctrl Pts',(11.1454425256572,8.04642571042556,6.15376086042613));
#15716=CARTESIAN_POINT('Ctrl Pts',(12.3775312688656,8.62595695949776,7.20723494454326));
#15717=CARTESIAN_POINT('Ctrl Pts',(13.7465187613193,9.269880569578,8.3777617046734));
#15718=CARTESIAN_POINT('Ctrl Pts',(14.2941137583009,9.52745001361009,8.84597240872545));
#15719=CARTESIAN_POINT('Ctrl Pts',(14.8417087552824,9.78501945764218,9.31418311277751));
#15720=CARTESIAN_POINT('Ctrl Pts',(15.3208543776412,10.0103927211703,9.72386747882306));
#15721=CARTESIAN_POINT('Ctrl Pts',(15.5946518761319,10.1391774431863,9.95797283084909));
#15722=CARTESIAN_POINT('Ctrl Pts',(15.7315506253773,10.2035698041943,10.0750255068621));
#15723=CARTESIAN_POINT('Ctrl Pts',(15.8,10.2357659846983,10.1335518448686));
#15724=CARTESIAN_POINT('Ctrl Pts',(15.8,10.2694450138623,10.160938779711));
#15725=CARTESIAN_POINT('Ctrl Pts',(15.8,10.2627800357942,10.1553950350833));
#15726=CARTESIAN_POINT('Ctrl Pts',(15.8,10.2560796357392,10.1498844772774));
#15727=CARTESIAN_POINT('Ctrl Pts',(15.8,10.2493438236809,10.1444070962816));
#15728=CARTESIAN_POINT('Ctrl Pts',(15.8,10.242572606579,10.1389628855307));
#15729=CARTESIAN_POINT('Ctrl Pts',(15.8,10.2357659846983,10.1335518448686));
#15730=CARTESIAN_POINT('Origin',(15.8,9.70545143020505,11.5149238208745));
#15731=CARTESIAN_POINT('Ctrl Pts',(10.0502525316942,9.86553218952113,4.2975012308678));
#15732=CARTESIAN_POINT('Ctrl Pts',(11.9668350211294,11.2772850923971,5.98055897313701));
#15733=CARTESIAN_POINT('Ctrl Pts',(13.8834175105647,12.689037995273,7.66361671540623));
#15734=CARTESIAN_POINT('Ctrl Pts',(15.8,14.1007908981489,9.34667445767544));
#15735=CARTESIAN_POINT('Ctrl Pts',(10.0502525316942,9.92430165934404,4.02946472694721));
#15736=CARTESIAN_POINT('Ctrl Pts',(11.9668350211294,11.3702854403574,5.67542688932036));
#15737=CARTESIAN_POINT('Ctrl Pts',(13.8834175105647,12.8166324188796,7.32120731702057));
#15738=CARTESIAN_POINT('Ctrl Pts',(15.8,14.262616199893,8.96716947939373));
#15739=CARTESIAN_POINT('Ctrl Pts',(10.0502525316942,9.97045860619055,3.61211062987325));
#15740=CARTESIAN_POINT('Ctrl Pts',(11.9668350211294,11.4635526451079,5.19299729643612));
#15741=CARTESIAN_POINT('Ctrl Pts',(13.8834175105647,12.956112555571,6.77411605990067));
#15742=CARTESIAN_POINT('Ctrl Pts',(15.8,14.4492065944883,8.35500272646354));
#15743=CARTESIAN_POINT('Ctrl Pts',(10.0502525316942,9.86609404202409,3.40259706500424));
#15744=CARTESIAN_POINT('Ctrl Pts',(11.9668350211294,11.3629139742223,4.93192196434908));
#15745=CARTESIAN_POINT('Ctrl Pts',(13.8834175105647,12.8596985741914,6.4612970474202));
#15746=CARTESIAN_POINT('Ctrl Pts',(15.8,14.3565185063896,7.99062194676504));
#15747=CARTESIAN_POINT('Ctrl Pts',(10.0502525316942,9.77087387154055,3.30601090928165));
#15748=CARTESIAN_POINT('Ctrl Pts',(11.9668350211295,11.2600017151873,4.80688444200922));
#15749=CARTESIAN_POINT('Ctrl Pts',(13.8834175105647,12.7494883087274,6.30755492143114));
#15750=CARTESIAN_POINT('Ctrl Pts',(15.8,14.2386161523742,7.8084284541587));
#15751=CARTESIAN_POINT('Ctrl Pts',(10.0502525316942,9.7053049496755,3.24522078037662));
#15752=CARTESIAN_POINT('Ctrl Pts',(11.9668350211294,11.1883166806211,4.72781700580775));
#15753=CARTESIAN_POINT('Ctrl Pts',(13.8834175105647,12.6715703878316,6.21037804061048));
#15754=CARTESIAN_POINT('Ctrl Pts',(15.8,14.1545821187772,7.69297426604161));
#15755=CARTESIAN_POINT('Ctrl Pts',(10.0502525316942,9.59290229251195,3.13558852137588));
#15756=CARTESIAN_POINT('Ctrl Pts',(11.9668350211294,11.0646742694966,4.58744122478927));
#15757=CARTESIAN_POINT('Ctrl Pts',(13.8834175105647,12.5366026187688,6.03905717649215));
#15758=CARTESIAN_POINT('Ctrl Pts',(15.8,14.0083745957535,7.49090987990554));
#15759=CARTESIAN_POINT('Ctrl Pts',(10.0502525316942,9.41310152025599,2.92757116168119));
#15760=CARTESIAN_POINT('Ctrl Pts',(11.9668350211294,10.8702564567215,4.32424671627921));
#15761=CARTESIAN_POINT('Ctrl Pts',(13.8834175105647,12.3275956094625,5.72097159497831));
#15762=CARTESIAN_POINT('Ctrl Pts',(15.8,13.784750545928,7.11764714957634));
#15763=CARTESIAN_POINT('Ctrl Pts',(10.0502525316942,9.19740926566326,2.78894862571459));
#15764=CARTESIAN_POINT('Ctrl Pts',(11.9668350211294,10.6275127538178,4.13765656795514));
#15765=CARTESIAN_POINT('Ctrl Pts',(13.8834175105647,12.0577280234799,5.48632659127462));
#15766=CARTESIAN_POINT('Ctrl Pts',(15.8,13.4878315116344,6.83503453351516));
#15767=CARTESIAN_POINT('Ctrl Pts',(10.0502525316942,8.97469639188219,2.6831512960299));
#15768=CARTESIAN_POINT('Ctrl Pts',(11.9668350211294,10.3719655284903,3.99115284441714));
#15769=CARTESIAN_POINT('Ctrl Pts',(13.8834175105647,11.7692966119437,5.29909475352163));
#15770=CARTESIAN_POINT('Ctrl Pts',(15.8,13.1665657485518,6.60709630190886));
#15771=CARTESIAN_POINT('Ctrl Pts',(10.0502525316942,8.85625319397989,2.64958522759924));
#15772=CARTESIAN_POINT('Ctrl Pts',(11.9668350211294,10.2341088589535,3.9399468856208));
#15773=CARTESIAN_POINT('Ctrl Pts',(13.8834175105647,11.612095695752,5.23040962052305));
#15774=CARTESIAN_POINT('Ctrl Pts',(15.8,12.9899513607256,6.52077127854461));
#15775=CARTESIAN_POINT('Ctrl Pts',(10.0502525316942,8.77492596468499,2.63468906623289));
#15776=CARTESIAN_POINT('Ctrl Pts',(11.9668350211294,10.1386945339445,3.91464433600868));
#15777=CARTESIAN_POINT('Ctrl Pts',(13.8834175105647,11.5024631032041,5.19459960578447));
#15778=CARTESIAN_POINT('Ctrl Pts',(15.8,12.8662316724636,6.47455487556026));
#15779=CARTESIAN_POINT('Ctrl Pts',(15.8,12.9067253609027,6.49019400603778));
#15780=CARTESIAN_POINT('Ctrl Pts',(15.8,12.8986734787776,6.48698118307512));
#15781=CARTESIAN_POINT('Ctrl Pts',(15.8,12.890598163633,6.48381086865141));
#15782=CARTESIAN_POINT('Ctrl Pts',(15.8,12.8824994218701,6.48068305016015));
#15783=CARTESIAN_POINT('Ctrl Pts',(15.8,12.874377258079,6.47759771920651));
#15784=CARTESIAN_POINT('Ctrl Pts',(15.8,12.8662316724636,6.47455487556026));
#15785=CARTESIAN_POINT('Origin',(15.8,12.7887399758658,7.95219390447097));
#15786=CARTESIAN_POINT('Ctrl Pts',(10.0502525316942,10.7106795892491,1.03854944428815));
#15787=CARTESIAN_POINT('Ctrl Pts',(11.9668350211294,12.5734298318033,2.20297683852746));
#15788=CARTESIAN_POINT('Ctrl Pts',(13.8834175105647,14.4361800743576,3.36740423276678));
#15789=CARTESIAN_POINT('Ctrl Pts',(15.8,16.2989303169119,4.5318316270061));
#15790=CARTESIAN_POINT('Ctrl Pts',(10.0502525316942,10.6837448416591,0.765470815703815));
#15791=CARTESIAN_POINT('Ctrl Pts',(11.9668350211294,12.5675874193204,1.88404029388038));
#15792=CARTESIAN_POINT('Ctrl Pts',(13.8834175105647,14.4517192592367,3.00232469790949));
#15793=CARTESIAN_POINT('Ctrl Pts',(15.8,16.335561836898,4.12089417608606));
#15794=CARTESIAN_POINT('Ctrl Pts',(10.0502525316942,10.5986742216641,0.354275884655605));
#15795=CARTESIAN_POINT('Ctrl Pts',(11.9668350211295,12.5072118829665,1.39639701818897));
#15796=CARTESIAN_POINT('Ctrl Pts',(13.8834175105647,14.4153151096237,2.43890221878173));
#15797=CARTESIAN_POINT('Ctrl Pts',(15.8,16.3238527709261,3.48102335231509));
#15798=CARTESIAN_POINT('Ctrl Pts',(10.0502525316942,10.4346757823309,0.187261072828499));
#15799=CARTESIAN_POINT('Ctrl Pts',(11.9668350211295,12.3308235163868,1.17919268731443));
#15800=CARTESIAN_POINT('Ctrl Pts',(13.8834175105647,14.2269575174279,2.17117887432507));
#15801=CARTESIAN_POINT('Ctrl Pts',(15.8,16.1231052514838,3.16311048881099));
#15802=CARTESIAN_POINT('Ctrl Pts',(10.0502525316942,10.3142698682631,0.124824203483034));
#15803=CARTESIAN_POINT('Ctrl Pts',(11.9668350211295,12.1943100355803,1.09207394643473));
#15804=CARTESIAN_POINT('Ctrl Pts',(13.8834175105647,14.0746341437949,2.05901454824882));
#15805=CARTESIAN_POINT('Ctrl Pts',(15.8,15.9546743111122,3.02626429120052));
#15806=CARTESIAN_POINT('Ctrl Pts',(10.0502525316942,10.2331249635989,0.0872711810328567));
#15807=CARTESIAN_POINT('Ctrl Pts',(11.9668350211295,12.1017003635113,1.03902815454411));
#15808=CARTESIAN_POINT('Ctrl Pts',(13.8834175105647,13.9705005205662,1.99067177195528));
#15809=CARTESIAN_POINT('Ctrl Pts',(15.8,15.8390759204785,2.94242874546654));
#15810=CARTESIAN_POINT('Ctrl Pts',(10.0502525316942,10.09234540735,0.0177390798696556));
#15811=CARTESIAN_POINT('Ctrl Pts',(11.9668350211294,11.9407308952458,0.943730501418608));
#15812=CARTESIAN_POINT('Ctrl Pts',(13.8834175105647,13.789197555515,1.86944300220409));
#15813=CARTESIAN_POINT('Ctrl Pts',(15.8,15.6375830434108,2.79543442375304));
#15814=CARTESIAN_POINT('Ctrl Pts',(10.0502525316942,9.85706386916291,-0.124535428292432));
#15815=CARTESIAN_POINT('Ctrl Pts',(11.9668350211295,11.6744970487389,0.753496320252986));
#15816=CARTESIAN_POINT('Ctrl Pts',(13.8834175105647,13.4921256030567,1.6315141640905));
#15817=CARTESIAN_POINT('Ctrl Pts',(15.8,15.3095587826327,2.50954591263591));
#15818=CARTESIAN_POINT('Ctrl Pts',(10.0502525316942,9.60909091476054,-0.189717758784554));
#15819=CARTESIAN_POINT('Ctrl Pts',(11.9668350211294,11.3859738307471,0.651053436707716));
#15820=CARTESIAN_POINT('Ctrl Pts',(13.8834175105647,13.1629551482145,1.49175101418763));
#15821=CARTESIAN_POINT('Ctrl Pts',(15.8,14.9398380642011,2.3325222096799));
#15822=CARTESIAN_POINT('Ctrl Pts',(10.0502525316942,9.36458479377687,-0.221513186022212));
#15823=CARTESIAN_POINT('Ctrl Pts',(11.9668350211294,11.0976614182865,0.59069030096811));
#15824=CARTESIAN_POINT('Ctrl Pts',(13.8834175105648,12.8307816497324,1.40281548080796));
#15825=CARTESIAN_POINT('Ctrl Pts',(15.8,14.563858274242,2.21501896779828));
#15826=CARTESIAN_POINT('Ctrl Pts',(10.0502525316942,9.24156417346731,-0.216827447239559));
#15827=CARTESIAN_POINT('Ctrl Pts',(11.9668350211294,10.9507264633732,0.584598599726621));
#15828=CARTESIAN_POINT('Ctrl Pts',(13.8834175105647,12.6600447395717,1.38608024219576));
#15829=CARTESIAN_POINT('Ctrl Pts',(15.8,14.3692070294775,2.18750628916194));
#15830=CARTESIAN_POINT('Ctrl Pts',(10.0502525316942,9.15961421508102,-0.20586304261726));
#15831=CARTESIAN_POINT('Ctrl Pts',(11.9668350211294,10.8521631299943,0.590019092973717));
#15832=CARTESIAN_POINT('Ctrl Pts',(13.8834175105647,12.5447120449076,1.38590122856469));
#15833=CARTESIAN_POINT('Ctrl Pts',(15.8,14.2372609598209,2.18178336415567));
#15834=CARTESIAN_POINT('Ctrl Pts',(15.8,14.2806055031745,2.18414382321291));
#15835=CARTESIAN_POINT('Ctrl Pts',(15.8,14.2719548913156,2.18357641541193));
#15836=CARTESIAN_POINT('Ctrl Pts',(15.8,14.2632951291918,2.18305667683518));
#15837=CARTESIAN_POINT('Ctrl Pts',(15.8,14.2546262189952,2.18258459351507));
#15838=CARTESIAN_POINT('Ctrl Pts',(15.8,14.2459481624974,2.18216015604922));
#15839=CARTESIAN_POINT('Ctrl Pts',(15.8,14.2372609598209,2.18178336415567));
#15840=CARTESIAN_POINT('Origin',(15.8,14.6201775482978,3.61104784250494));
#15841=CARTESIAN_POINT('Origin',(21.,10.,0.));
#15842=CARTESIAN_POINT('',(0.,0.,0.));
#15843=CARTESIAN_POINT('Origin',(24.5,-9.875,0.));
#15844=CARTESIAN_POINT('',(22.2,-10.,0.));
#15845=CARTESIAN_POINT('',(24.5,-9.78106229945361,2.08106229945361));
#15846=CARTESIAN_POINT('Ctrl Pts',(22.2,-10.,-3.46944695195361E-17));
#15847=CARTESIAN_POINT('Ctrl Pts',(22.2,-10.,0.279281663145492));
#15848=CARTESIAN_POINT('Ctrl Pts',(22.2664319537276,-9.98711221417022,0.57235161892421));
#15849=CARTESIAN_POINT('Ctrl Pts',(22.5234308581959,-9.94287664809831,1.09963640431428));
#15850=CARTESIAN_POINT('Ctrl Pts',(22.7136761128309,-9.91228969341567,1.33407151029786));
#15851=CARTESIAN_POINT('Ctrl Pts',(23.1318392128932,-9.8577299734025,1.69022028358443));
#15852=CARTESIAN_POINT('Ctrl Pts',(23.3865793433932,-9.82998540360157,1.83883276387722));
#15853=CARTESIAN_POINT('Ctrl Pts',(23.9342975404997,-9.79141246827269,2.03424683169264));
#15854=CARTESIAN_POINT('Ctrl Pts',(24.2273042269987,-9.78106229945361,2.08106229945361));
#15855=CARTESIAN_POINT('Ctrl Pts',(24.5,-9.78106229945361,2.08106229945361));
#15856=CARTESIAN_POINT('',(26.8,-10.,0.));
#15857=CARTESIAN_POINT('Ctrl Pts',(26.8,-10.,1.04083408558608E-15));
#15858=CARTESIAN_POINT('Ctrl Pts',(26.8,-10.,-0.279281663145491));
#15859=CARTESIAN_POINT('Ctrl Pts',(26.7335680462724,-9.98711221417022,-0.57235161892421));
#15860=CARTESIAN_POINT('Ctrl Pts',(26.4765691418041,-9.94287664809831,-1.09963640431428));
#15861=CARTESIAN_POINT('Ctrl Pts',(26.2863238871692,-9.91228969341567,-1.33407151029786));
#15862=CARTESIAN_POINT('Ctrl Pts',(25.8681607871068,-9.8577299734025,-1.69022028358443));
#15863=CARTESIAN_POINT('Ctrl Pts',(25.6134206566068,-9.82998540360157,-1.83883276387722));
#15864=CARTESIAN_POINT('Ctrl Pts',(25.0657024595003,-9.79141246827269,-2.03424683169264));
#15865=CARTESIAN_POINT('Ctrl Pts',(24.7726957730013,-9.78106229945362,-2.08106229945361));
#15866=CARTESIAN_POINT('Ctrl Pts',(24.5,-9.78106229945362,-2.08106229945361));
#15867=CARTESIAN_POINT('Ctrl Pts',(24.2273042269987,-9.78106229945362,-2.08106229945361));
#15868=CARTESIAN_POINT('Ctrl Pts',(23.9342975404997,-9.79141246827269,-2.03424683169264));
#15869=CARTESIAN_POINT('Ctrl Pts',(23.3865793433932,-9.82998540360157,-1.83883276387722));
#15870=CARTESIAN_POINT('Ctrl Pts',(23.1318392128932,-9.8577299734025,-1.69022028358443));
#15871=CARTESIAN_POINT('Ctrl Pts',(22.7136761128309,-9.91228969341567,-1.33407151029786));
#15872=CARTESIAN_POINT('Ctrl Pts',(22.5234308581959,-9.94287664809831,-1.09963640431428));
#15873=CARTESIAN_POINT('Ctrl Pts',(22.2664319537276,-9.98711221417022,-0.572351618924211));
#15874=CARTESIAN_POINT('Ctrl Pts',(22.2,-10.,-0.279281663145492));
#15875=CARTESIAN_POINT('Ctrl Pts',(22.2,-10.,4.85722573273506E-16));
#15876=CARTESIAN_POINT('Ctrl Pts',(24.5,-9.78106229945361,2.08106229945361));
#15877=CARTESIAN_POINT('Ctrl Pts',(24.7726957730013,-9.78106229945361,2.08106229945361));
#15878=CARTESIAN_POINT('Ctrl Pts',(25.0657024595003,-9.79141246827269,2.03424683169264));
#15879=CARTESIAN_POINT('Ctrl Pts',(25.6134206566068,-9.82998540360157,1.83883276387722));
#15880=CARTESIAN_POINT('Ctrl Pts',(25.8681607871068,-9.8577299734025,1.69022028358443));
#15881=CARTESIAN_POINT('Ctrl Pts',(26.2863238871692,-9.91228969341567,1.33407151029786));
#15882=CARTESIAN_POINT('Ctrl Pts',(26.4765691418041,-9.94287664809831,1.09963640431428));
#15883=CARTESIAN_POINT('Ctrl Pts',(26.7335680462724,-9.98711221417022,0.572351618924211));
#15884=CARTESIAN_POINT('Ctrl Pts',(26.8,-10.,0.279281663145492));
#15885=CARTESIAN_POINT('Ctrl Pts',(26.8,-10.,-2.08166817117217E-16));
#15886=CARTESIAN_POINT('',(24.5,-9.75,2.05));
#15887=CARTESIAN_POINT('',(24.5,-9.875,2.175));
#15888=CARTESIAN_POINT('Origin',(24.5,-9.75,0.));
#15889=CARTESIAN_POINT('Origin',(24.5,-7.75,0.));
#15890=CARTESIAN_POINT('',(24.5,-5.66552071746278,2.05));
#15891=CARTESIAN_POINT('',(24.5,-7.75,2.05));
#15892=CARTESIAN_POINT('',(26.55,-6.025,-3.34230378723604E-16));
#15893=CARTESIAN_POINT('Ctrl Pts',(26.55,-6.025,1.38777878078145E-16));
#15894=CARTESIAN_POINT('Ctrl Pts',(26.55,-6.025,0.259594733817565));
#15895=CARTESIAN_POINT('Ctrl Pts',(26.4976983668916,-6.00658123724956,0.535111320788412));
#15896=CARTESIAN_POINT('Ctrl Pts',(26.287830413716,-5.94008056213222,1.03961781502895));
#15897=CARTESIAN_POINT('Ctrl Pts',(26.13037388806,-5.8928399020443,1.26876391480488));
#15898=CARTESIAN_POINT('Ctrl Pts',(25.7686724003374,-5.80318375449856,1.63046540252745));
#15899=CARTESIAN_POINT('Ctrl Pts',(25.5395625840329,-5.75468697285078,1.78785157007388));
#15900=CARTESIAN_POINT('Ctrl Pts',(25.035191264494,-5.68525838031662,1.99766693028397));
#15901=CARTESIAN_POINT('Ctrl Pts',(24.7597261277258,-5.66552071746278,2.05));
#15902=CARTESIAN_POINT('Ctrl Pts',(24.5,-5.66552071746278,2.05));
#15903=CARTESIAN_POINT('',(22.45,-6.025,-6.81175073918965E-16));
#15904=CARTESIAN_POINT('Ctrl Pts',(22.45,-6.025,-6.24500451351651E-16));
#15905=CARTESIAN_POINT('Ctrl Pts',(22.45,-6.025,-0.259594733817566));
#15906=CARTESIAN_POINT('Ctrl Pts',(22.5023016331084,-6.00658123724956,-0.535111320788414));
#15907=CARTESIAN_POINT('Ctrl Pts',(22.712169586284,-5.94008056213222,-1.03961781502895));
#15908=CARTESIAN_POINT('Ctrl Pts',(22.86962611194,-5.8928399020443,-1.26876391480488));
#15909=CARTESIAN_POINT('Ctrl Pts',(23.2313275996626,-5.80318375449856,-1.63046540252745));
#15910=CARTESIAN_POINT('Ctrl Pts',(23.4604374159671,-5.75468697285078,-1.78785157007388));
#15911=CARTESIAN_POINT('Ctrl Pts',(23.964808735506,-5.68525838031662,-1.99766693028397));
#15912=CARTESIAN_POINT('Ctrl Pts',(24.2402738722742,-5.66552071746278,-2.05));
#15913=CARTESIAN_POINT('Ctrl Pts',(24.7597261277258,-5.66552071746278,-2.05));
#15914=CARTESIAN_POINT('Ctrl Pts',(25.035191264494,-5.68525838031662,-1.99766693028397));
#15915=CARTESIAN_POINT('Ctrl Pts',(25.5395625840329,-5.75468697285078,-1.78785157007388));
#15916=CARTESIAN_POINT('Ctrl Pts',(25.7686724003374,-5.80318375449856,-1.63046540252745));
#15917=CARTESIAN_POINT('Ctrl Pts',(26.13037388806,-5.8928399020443,-1.26876391480488));
#15918=CARTESIAN_POINT('Ctrl Pts',(26.287830413716,-5.94008056213222,-1.03961781502895));
#15919=CARTESIAN_POINT('Ctrl Pts',(26.4976983668916,-6.00658123724956,-0.535111320788414));
#15920=CARTESIAN_POINT('Ctrl Pts',(26.55,-6.025,-0.259594733817566));
#15921=CARTESIAN_POINT('Ctrl Pts',(26.55,-6.025,-6.24500451351651E-16));
#15922=CARTESIAN_POINT('Ctrl Pts',(24.5,-5.66552071746278,2.05));
#15923=CARTESIAN_POINT('Ctrl Pts',(24.2402738722742,-5.66552071746278,2.05));
#15924=CARTESIAN_POINT('Ctrl Pts',(23.964808735506,-5.68525838031662,1.99766693028397));
#15925=CARTESIAN_POINT('Ctrl Pts',(23.4604374159671,-5.75468697285078,1.78785157007388));
#15926=CARTESIAN_POINT('Ctrl Pts',(23.2313275996626,-5.80318375449856,1.63046540252745));
#15927=CARTESIAN_POINT('Ctrl Pts',(22.86962611194,-5.8928399020443,1.26876391480488));
#15928=CARTESIAN_POINT('Ctrl Pts',(22.712169586284,-5.94008056213222,1.03961781502895));
#15929=CARTESIAN_POINT('Ctrl Pts',(22.5023016331084,-6.00658123724956,0.535111320788414));
#15930=CARTESIAN_POINT('Ctrl Pts',(22.45,-6.025,0.259594733817566));
#15931=CARTESIAN_POINT('Ctrl Pts',(22.45,-6.025,0.));
#15932=CARTESIAN_POINT('Origin',(24.5,0.,9.875));
#15933=CARTESIAN_POINT('',(22.2,0.,10.));
#15934=CARTESIAN_POINT('',(26.8,0.,10.));
#15935=CARTESIAN_POINT('Ctrl Pts',(22.2,-2.77555756156289E-16,10.));
#15936=CARTESIAN_POINT('Ctrl Pts',(22.2,0.279281663145492,10.));
#15937=CARTESIAN_POINT('Ctrl Pts',(22.2664319537276,0.57235161892421,9.98711221417022));
#15938=CARTESIAN_POINT('Ctrl Pts',(22.5234308581959,1.09963640431428,9.94287664809831));
#15939=CARTESIAN_POINT('Ctrl Pts',(22.7136761128309,1.33407151029786,9.91228969341567));
#15940=CARTESIAN_POINT('Ctrl Pts',(23.1318392128932,1.69022028358443,9.8577299734025));
#15941=CARTESIAN_POINT('Ctrl Pts',(23.3865793433932,1.83883276387722,9.82998540360157));
#15942=CARTESIAN_POINT('Ctrl Pts',(23.9342975404997,2.03424683169264,9.79141246827269));
#15943=CARTESIAN_POINT('Ctrl Pts',(24.2273042269987,2.08106229945361,9.78106229945362));
#15944=CARTESIAN_POINT('Ctrl Pts',(24.7726957730013,2.08106229945361,9.78106229945362));
#15945=CARTESIAN_POINT('Ctrl Pts',(25.0657024595003,2.03424683169264,9.79141246827269));
#15946=CARTESIAN_POINT('Ctrl Pts',(25.6134206566068,1.83883276387722,9.82998540360157));
#15947=CARTESIAN_POINT('Ctrl Pts',(25.8681607871068,1.69022028358443,9.8577299734025));
#15948=CARTESIAN_POINT('Ctrl Pts',(26.2863238871692,1.33407151029786,9.91228969341567));
#15949=CARTESIAN_POINT('Ctrl Pts',(26.4765691418041,1.09963640431428,9.94287664809831));
#15950=CARTESIAN_POINT('Ctrl Pts',(26.7335680462724,0.572351618924211,9.98711221417022));
#15951=CARTESIAN_POINT('Ctrl Pts',(26.8,0.279281663145492,10.));
#15952=CARTESIAN_POINT('Ctrl Pts',(26.8,0.,10.));
#15953=CARTESIAN_POINT('',(22.45,2.51052593825207E-16,9.75));
#15954=CARTESIAN_POINT('',(22.325,2.66360678814549E-16,9.875));
#15955=CARTESIAN_POINT('Origin',(24.5,0.,9.75));
#15956=CARTESIAN_POINT('Ctrl Pts',(26.8,1.31838984174237E-15,10.));
#15957=CARTESIAN_POINT('Ctrl Pts',(26.8,-0.279281663145491,10.));
#15958=CARTESIAN_POINT('Ctrl Pts',(26.7335680462724,-0.572351618924209,
9.98711221417022));
#15959=CARTESIAN_POINT('Ctrl Pts',(26.4765691418041,-1.09963640431428,9.94287664809831));
#15960=CARTESIAN_POINT('Ctrl Pts',(26.2863238871692,-1.33407151029786,9.91228969341567));
#15961=CARTESIAN_POINT('Ctrl Pts',(25.8681607871068,-1.69022028358443,9.8577299734025));
#15962=CARTESIAN_POINT('Ctrl Pts',(25.6134206566068,-1.83883276387722,9.82998540360157));
#15963=CARTESIAN_POINT('Ctrl Pts',(25.0657024595003,-2.03424683169264,9.79141246827269));
#15964=CARTESIAN_POINT('Ctrl Pts',(24.7726957730013,-2.08106229945361,9.78106229945362));
#15965=CARTESIAN_POINT('Ctrl Pts',(24.5,-2.08106229945361,9.78106229945362));
#15966=CARTESIAN_POINT('Ctrl Pts',(24.2273042269987,-2.08106229945361,9.78106229945362));
#15967=CARTESIAN_POINT('Ctrl Pts',(23.9342975404997,-2.03424683169264,9.79141246827269));
#15968=CARTESIAN_POINT('Ctrl Pts',(23.3865793433932,-1.83883276387722,9.82998540360157));
#15969=CARTESIAN_POINT('Ctrl Pts',(23.1318392128932,-1.69022028358443,9.8577299734025));
#15970=CARTESIAN_POINT('Ctrl Pts',(22.7136761128309,-1.33407151029786,9.91228969341567));
#15971=CARTESIAN_POINT('Ctrl Pts',(22.5234308581959,-1.09963640431428,9.94287664809831));
#15972=CARTESIAN_POINT('Ctrl Pts',(22.2664319537276,-0.572351618924211,
9.98711221417022));
#15973=CARTESIAN_POINT('Ctrl Pts',(22.2,-0.279281663145492,10.));
#15974=CARTESIAN_POINT('Ctrl Pts',(22.2,3.46944695195361E-16,10.));
#15975=CARTESIAN_POINT('Origin',(24.5,0.,7.75));
#15976=CARTESIAN_POINT('',(22.45,1.94915235951676E-16,6.025));
#15977=CARTESIAN_POINT('',(22.45,2.51052593825207E-16,7.75));
#15978=CARTESIAN_POINT('',(24.5,2.05,5.66552071746278));
#15979=CARTESIAN_POINT('Ctrl Pts',(24.5,2.05,5.66552071746278));
#15980=CARTESIAN_POINT('Ctrl Pts',(24.2402738722742,2.05,5.66552071746278));
#15981=CARTESIAN_POINT('Ctrl Pts',(23.964808735506,1.99766693028397,5.68525838031662));
#15982=CARTESIAN_POINT('Ctrl Pts',(23.4604374159671,1.78785157007388,5.75468697285078));
#15983=CARTESIAN_POINT('Ctrl Pts',(23.2313275996626,1.63046540252745,5.80318375449856));
#15984=CARTESIAN_POINT('Ctrl Pts',(22.86962611194,1.26876391480488,5.8928399020443));
#15985=CARTESIAN_POINT('Ctrl Pts',(22.712169586284,1.03961781502895,5.94008056213222));
#15986=CARTESIAN_POINT('Ctrl Pts',(22.5023016331084,0.535111320788414,6.00658123724956));
#15987=CARTESIAN_POINT('Ctrl Pts',(22.45,0.259594733817566,6.025));
#15988=CARTESIAN_POINT('Ctrl Pts',(22.45,2.77555756156289E-16,6.025));
#15989=CARTESIAN_POINT('Ctrl Pts',(22.45,2.08166817117217E-16,6.025));
#15990=CARTESIAN_POINT('Ctrl Pts',(22.45,-0.259594733817565,6.025));
#15991=CARTESIAN_POINT('Ctrl Pts',(22.5023016331084,-0.535111320788413,
6.00658123724956));
#15992=CARTESIAN_POINT('Ctrl Pts',(22.712169586284,-1.03961781502895,5.94008056213222));
#15993=CARTESIAN_POINT('Ctrl Pts',(22.86962611194,-1.26876391480488,5.8928399020443));
#15994=CARTESIAN_POINT('Ctrl Pts',(23.2313275996626,-1.63046540252745,5.80318375449856));
#15995=CARTESIAN_POINT('Ctrl Pts',(23.4604374159671,-1.78785157007388,5.75468697285078));
#15996=CARTESIAN_POINT('Ctrl Pts',(23.964808735506,-1.99766693028397,5.68525838031662));
#15997=CARTESIAN_POINT('Ctrl Pts',(24.2402738722742,-2.05,5.66552071746278));
#15998=CARTESIAN_POINT('Ctrl Pts',(24.7597261277258,-2.05,5.66552071746278));
#15999=CARTESIAN_POINT('Ctrl Pts',(25.035191264494,-1.99766693028397,5.68525838031662));
#16000=CARTESIAN_POINT('Ctrl Pts',(25.5395625840329,-1.78785157007388,5.75468697285078));
#16001=CARTESIAN_POINT('Ctrl Pts',(25.7686724003374,-1.63046540252745,5.80318375449856));
#16002=CARTESIAN_POINT('Ctrl Pts',(26.13037388806,-1.26876391480488,5.8928399020443));
#16003=CARTESIAN_POINT('Ctrl Pts',(26.287830413716,-1.03961781502895,5.94008056213222));
#16004=CARTESIAN_POINT('Ctrl Pts',(26.4976983668916,-0.535111320788413,
6.00658123724956));
#16005=CARTESIAN_POINT('Ctrl Pts',(26.55,-0.259594733817566,6.025));
#16006=CARTESIAN_POINT('Ctrl Pts',(26.55,0.259594733817565,6.025));
#16007=CARTESIAN_POINT('Ctrl Pts',(26.4976983668916,0.535111320788412,6.00658123724956));
#16008=CARTESIAN_POINT('Ctrl Pts',(26.287830413716,1.03961781502895,5.94008056213222));
#16009=CARTESIAN_POINT('Ctrl Pts',(26.13037388806,1.26876391480488,5.8928399020443));
#16010=CARTESIAN_POINT('Ctrl Pts',(25.7686724003374,1.63046540252745,5.80318375449856));
#16011=CARTESIAN_POINT('Ctrl Pts',(25.5395625840329,1.78785157007388,5.75468697285078));
#16012=CARTESIAN_POINT('Ctrl Pts',(25.035191264494,1.99766693028397,5.68525838031662));
#16013=CARTESIAN_POINT('Ctrl Pts',(24.7597261277258,2.05,5.66552071746278));
#16014=CARTESIAN_POINT('Ctrl Pts',(24.5,2.05,5.66552071746278));
#16015=CARTESIAN_POINT('Origin',(10.3002525316942,0.,0.));
#16016=CARTESIAN_POINT('',(10.0502525316942,6.525,-7.99082036443648E-16));
#16017=CARTESIAN_POINT('Origin',(10.0502525316942,0.,0.));
#16018=CARTESIAN_POINT('',(10.5502525316942,6.025,7.3784969648628E-16));
#16019=CARTESIAN_POINT('',(10.3002525316942,6.275,-7.68465866464964E-16));
#16020=CARTESIAN_POINT('',(10.5502525316942,-6.025,-7.3784969648628E-16));
#16021=CARTESIAN_POINT('Origin',(10.5502525316942,0.,0.));
#16022=CARTESIAN_POINT('Origin',(10.5502525316942,0.,0.));
#16023=CARTESIAN_POINT('Origin',(19.7001262658471,0.,0.));
#16024=CARTESIAN_POINT('',(28.85,6.025,-7.3784969648628E-16));
#16025=CARTESIAN_POINT('',(28.85,-6.025,-7.3784969648628E-16));
#16026=CARTESIAN_POINT('Origin',(28.85,0.,0.));
#16027=CARTESIAN_POINT('Origin',(28.85,0.,0.));
#16028=CARTESIAN_POINT('',(19.7001262658471,-6.025,-7.3784969648628E-16));
#16029=CARTESIAN_POINT('',(19.7001262658471,-6.025,-7.3784969648628E-16));
#16030=CARTESIAN_POINT('Origin',(10.0502525316942,9.16192731696939,0.));
#16031=CARTESIAN_POINT('',(10.0502525316942,8.25473589028142,-3.97495252086484));
#16032=CARTESIAN_POINT('',(10.0502525316942,8.69919410795919,-2.87487982939776));
#16033=CARTESIAN_POINT('Origin',(10.0502525316942,0.,0.));
#16034=CARTESIAN_POINT('',(10.0502525316942,9.36936257048691,-5.29266352931554));
#16035=CARTESIAN_POINT('Ctrl Pts',(10.0502525316942,8.25473589028142,-3.97495252086484));
#16036=CARTESIAN_POINT('Ctrl Pts',(10.0502525316942,8.26501573550299,-3.9787354050507));
#16037=CARTESIAN_POINT('Ctrl Pts',(10.0502525316942,8.28548315894707,-3.98649262817573));
#16038=CARTESIAN_POINT('Ctrl Pts',(10.0502525316942,8.31590749387114,-3.9987028261882));
#16039=CARTESIAN_POINT('Ctrl Pts',(10.0502525316942,8.35591866443433,-4.01613390483614));
#16040=CARTESIAN_POINT('Ctrl Pts',(10.0502525316942,8.40499831559484,-4.03985675684261));
#16041=CARTESIAN_POINT('Ctrl Pts',(10.0502525316942,8.45312379306447,-4.06554061525075));
#16042=CARTESIAN_POINT('Ctrl Pts',(10.0502525316942,8.50026327435046,-4.09322319459339));
#16043=CARTESIAN_POINT('Ctrl Pts',(10.0502525316942,8.54637031220843,-4.12295311857557));
#16044=CARTESIAN_POINT('Ctrl Pts',(10.0502525316942,8.59138312702269,-4.1547878023559));
#16045=CARTESIAN_POINT('Ctrl Pts',(10.0502525316942,8.63523937649908,-4.18877458937294));
#16046=CARTESIAN_POINT('Ctrl Pts',(10.0502525316942,8.67789021323112,-4.22493224148239));
#16047=CARTESIAN_POINT('Ctrl Pts',(10.0502525316942,8.71931397871314,-4.26323309731516));
#16048=CARTESIAN_POINT('Ctrl Pts',(10.0502525316942,8.75953271831989,-4.30358079311506));
#16049=CARTESIAN_POINT('Ctrl Pts',(10.0502525316942,8.79862131584184,-4.34579910040493));
#16050=CARTESIAN_POINT('Ctrl Pts',(10.0502525316942,8.83668400083504,-4.38966981967219));
#16051=CARTESIAN_POINT('Ctrl Pts',(10.0502525316942,8.87383549938658,-4.43496376972659));
#16052=CARTESIAN_POINT('Ctrl Pts',(10.0502525316942,8.91018166484712,-4.48147234048105));
#16053=CARTESIAN_POINT('Ctrl Pts',(10.0502525316942,8.94579828347148,-4.52904236806123));
#16054=CARTESIAN_POINT('Ctrl Pts',(10.0502525316942,8.98071755670482,-4.57759789799494));
#16055=CARTESIAN_POINT('Ctrl Pts',(10.0502525316942,9.01494291264748,-4.62711375721922));
#16056=CARTESIAN_POINT('Ctrl Pts',(10.0502525316942,9.04845937030362,-4.67759669462988));
#16057=CARTESIAN_POINT('Ctrl Pts',(10.0502525316942,9.08124522426278,-4.72906440450668));
#16058=CARTESIAN_POINT('Ctrl Pts',(10.0502525316942,9.11328422214026,-4.78152352641848));
#16059=CARTESIAN_POINT('Ctrl Pts',(10.0502525316942,9.14457471976904,-4.83495345882569));
#16060=CARTESIAN_POINT('Ctrl Pts',(10.0502525316942,9.17512453503235,-4.88931713153334));
#16061=CARTESIAN_POINT('Ctrl Pts',(10.0502525316942,9.20494811701998,-4.9445675341018));
#16062=CARTESIAN_POINT('Ctrl Pts',(10.0502525316942,9.23406306612411,-5.00065547708482));
#16063=CARTESIAN_POINT('Ctrl Pts',(10.0502525316942,9.26248702510056,-5.05753691650348));
#16064=CARTESIAN_POINT('Ctrl Pts',(10.0502525316942,9.29023486488122,-5.11517936005741));
#16065=CARTESIAN_POINT('Ctrl Pts',(10.0502525316942,9.31731853484592,-5.17355993514958));
#16066=CARTESIAN_POINT('Ctrl Pts',(10.0502525316942,9.33846108530483,-5.22084339412737));
#16067=CARTESIAN_POINT('Ctrl Pts',(10.0502525316942,9.35402540755351,-5.25662833187234));
#16068=CARTESIAN_POINT('Ctrl Pts',(10.0502525316942,9.3642718170601,-5.28062796260048));
#16069=CARTESIAN_POINT('Ctrl Pts',(10.0502525316942,9.36936257048691,-5.29266352931554));
#16070=CARTESIAN_POINT('',(10.0502525316942,7.38503851882133,-5.42237201204004));
#16071=CARTESIAN_POINT('Ctrl Pts',(10.0502525316942,9.36936257048691,-5.29266352931554));
#16072=CARTESIAN_POINT('Ctrl Pts',(10.0502525316942,9.34434525366385,-5.32181765856171));
#16073=CARTESIAN_POINT('Ctrl Pts',(10.0502525316942,9.29515286061949,-5.37803958295792));
#16074=CARTESIAN_POINT('Ctrl Pts',(10.0502525316942,9.22389100140796,-5.45611344595659));
#16075=CARTESIAN_POINT('Ctrl Pts',(10.0502525316942,9.13393772674446,-5.54767139923329));
#16076=CARTESIAN_POINT('Ctrl Pts',(10.0502525316942,9.02993079896417,-5.64122622022819));
#16077=CARTESIAN_POINT('Ctrl Pts',(10.0502525316942,8.93425530662678,-5.71414742300118));
#16078=CARTESIAN_POINT('Ctrl Pts',(10.0502525316942,8.84663552299331,-5.76712457531372));
#16079=CARTESIAN_POINT('Ctrl Pts',(10.0502525316942,8.76653902495464,-5.80148760154655));
#16080=CARTESIAN_POINT('Ctrl Pts',(10.0502525316942,8.69311263972367,-5.81936638407584));
#16081=CARTESIAN_POINT('Ctrl Pts',(10.0502525316942,8.62505870129886,-5.82399901560002));
#16082=CARTESIAN_POINT('Ctrl Pts',(10.0502525316942,8.56077284249031,-5.81938869186267));
#16083=CARTESIAN_POINT('Ctrl Pts',(10.0502525316942,8.4986070414541,-5.80964873807682));
#16084=CARTESIAN_POINT('Ctrl Pts',(10.0502525316942,8.43709945169241,-5.79843016859412));
#16085=CARTESIAN_POINT('Ctrl Pts',(10.0502525316942,8.37520120352267,-5.78835717995633));
#16086=CARTESIAN_POINT('Ctrl Pts',(10.0502525316942,8.31255178250645,-5.78034060190006));
#16087=CARTESIAN_POINT('Ctrl Pts',(10.0502525316942,8.24933415385039,-5.77394633717213));
#16088=CARTESIAN_POINT('Ctrl Pts',(10.0502525316942,8.18604879427487,-5.76796747841793));
#16089=CARTESIAN_POINT('Ctrl Pts',(10.0502525316942,8.12332066784839,-5.76091367696946));
#16090=CARTESIAN_POINT('Ctrl Pts',(10.0502525316942,8.06168961610356,-5.75154264947447));
#16091=CARTESIAN_POINT('Ctrl Pts',(10.0502525316942,8.00141929583747,-5.73934420595248));
#16092=CARTESIAN_POINT('Ctrl Pts',(10.0502525316942,7.94258074919088,-5.72431483522833));
#16093=CARTESIAN_POINT('Ctrl Pts',(10.0502525316942,7.88512587067823,-5.70675814390461));
#16094=CARTESIAN_POINT('Ctrl Pts',(10.0502525316942,7.82895914189736,-5.68709020402104));
#16095=CARTESIAN_POINT('Ctrl Pts',(10.0502525316942,7.77401905533046,-5.66561822174726));
#16096=CARTESIAN_POINT('Ctrl Pts',(10.0502525316942,7.72032292706671,-5.64241804293469));
#16097=CARTESIAN_POINT('Ctrl Pts',(10.0502525316942,7.6679311867486,-5.61742944592276));
#16098=CARTESIAN_POINT('Ctrl Pts',(10.0502525316942,7.61692741952956,-5.59050809253397));
#16099=CARTESIAN_POINT('Ctrl Pts',(10.0502525316942,7.56739405041849,-5.56148971316608));
#16100=CARTESIAN_POINT('Ctrl Pts',(10.0502525316942,7.51938467268366,-5.53026090613148));
#16101=CARTESIAN_POINT('Ctrl Pts',(10.0502525316942,7.47292244003411,-5.4967684895078));
#16102=CARTESIAN_POINT('Ctrl Pts',(10.0502525316942,7.43699488267859,-5.46814894648693));
#16103=CARTESIAN_POINT('Ctrl Pts',(10.0502525316942,7.41074614986957,-5.44565864507534));
#16104=CARTESIAN_POINT('Ctrl Pts',(10.0502525316942,7.39355619607562,-5.43021006317766));
#16105=CARTESIAN_POINT('Ctrl Pts',(10.0502525316942,7.38503851882133,-5.42237201204004));
#16106=CARTESIAN_POINT('',(10.0502525316942,6.62239247796684,-6.33125817110613));
#16107=CARTESIAN_POINT('Origin',(10.0502525316942,0.,0.));
#16108=CARTESIAN_POINT('',(10.0502525316942,7.27527035012649,-7.92891439885425));
#16109=CARTESIAN_POINT('Ctrl Pts',(10.0502525316942,6.62239247796684,-6.33125817110613));
#16110=CARTESIAN_POINT('Ctrl Pts',(10.0502525316942,6.63100021625014,-6.33803255463449));
#16111=CARTESIAN_POINT('Ctrl Pts',(10.0502525316942,6.64806877891362,-6.35173489391119));
#16112=CARTESIAN_POINT('Ctrl Pts',(10.0502525316942,6.67323088220656,-6.37274911883029));
#16113=CARTESIAN_POINT('Ctrl Pts',(10.0502525316942,6.70589726716278,-6.40169119143333));
#16114=CARTESIAN_POINT('Ctrl Pts',(10.0502525316942,6.74524402479143,-6.43941941070578));
#16115=CARTESIAN_POINT('Ctrl Pts',(10.0502525316942,6.7830773250095,-6.47871780200897));
#16116=CARTESIAN_POINT('Ctrl Pts',(10.0502525316942,6.81935524839631,-6.51961240030403));
#16117=CARTESIAN_POINT('Ctrl Pts',(10.0502525316942,6.85401859544624,-6.56213509649465));
#16118=CARTESIAN_POINT('Ctrl Pts',(10.0502525316942,6.88699086799345,-6.60632140469039));
#16119=CARTESIAN_POINT('Ctrl Pts',(10.0502525316942,6.91819814506577,-6.65219708634863));
#16120=CARTESIAN_POINT('Ctrl Pts',(10.0502525316942,6.9475881722867,-6.69976489037577));
#16121=CARTESIAN_POINT('Ctrl Pts',(10.0502525316942,6.97514889902642,-6.74899181640015));
#16122=CARTESIAN_POINT('Ctrl Pts',(10.0502525316942,7.00093106972056,-6.79979302943897));
#16123=CARTESIAN_POINT('Ctrl Pts',(10.0502525316942,7.02506036068034,-6.85202406661451));
#16124=CARTESIAN_POINT('Ctrl Pts',(10.0502525316942,7.04770332746178,-6.90550961656264));
#16125=CARTESIAN_POINT('Ctrl Pts',(10.0502525316942,7.06903990194017,-6.96006716732954));
#16126=CARTESIAN_POINT('Ctrl Pts',(10.0502525316942,7.08923522069654,-7.01553102941681));
#16127=CARTESIAN_POINT('Ctrl Pts',(10.0502525316942,7.10840869098247,-7.07177895456439));
#16128=CARTESIAN_POINT('Ctrl Pts',(10.0502525316942,7.12661440941494,-7.12874865657033));
#16129=CARTESIAN_POINT('Ctrl Pts',(10.0502525316942,7.14386341521534,-7.18641725377035));
#16130=CARTESIAN_POINT('Ctrl Pts',(10.0502525316942,7.16013937508649,-7.24478653536347));
#16131=CARTESIAN_POINT('Ctrl Pts',(10.0502525316942,7.17541617812315,-7.30386662226907));
#16132=CARTESIAN_POINT('Ctrl Pts',(10.0502525316942,7.18967631564937,-7.36365880682929));
#16133=CARTESIAN_POINT('Ctrl Pts',(10.0502525316942,7.2029245901952,-7.42414298774012));
#16134=CARTESIAN_POINT('Ctrl Pts',(10.0502525316942,7.21517989232968,-7.48528632500984));
#16135=CARTESIAN_POINT('Ctrl Pts',(10.0502525316942,7.22647049097858,-7.54704857406782));
#16136=CARTESIAN_POINT('Ctrl Pts',(10.0502525316942,7.23682832548437,-7.60938839179095));
#16137=CARTESIAN_POINT('Ctrl Pts',(10.0502525316942,7.24628378544295,-7.67226934177745));
#16138=CARTESIAN_POINT('Ctrl Pts',(10.0502525316942,7.254861054624,-7.73566511738401));
#16139=CARTESIAN_POINT('Ctrl Pts',(10.0502525316942,7.26257856558425,-7.79955765803962));
#16140=CARTESIAN_POINT('Ctrl Pts',(10.0502525316942,7.26807493359233,-7.85106030720964));
#16141=CARTESIAN_POINT('Ctrl Pts',(10.0502525316942,7.27181932978281,-7.88990344551799));
#16142=CARTESIAN_POINT('Ctrl Pts',(10.0502525316942,7.27414795055896,-7.91589476537953));
#16143=CARTESIAN_POINT('Ctrl Pts',(10.0502525316942,7.27527035012649,-7.92891439885425));
#16144=CARTESIAN_POINT('',(10.0502525316942,5.34798390487229,-7.43908464225652));
#16145=CARTESIAN_POINT('Ctrl Pts',(10.0502525316942,7.27527035012649,-7.92891439885425));
#16146=CARTESIAN_POINT('Ctrl Pts',(10.0502525316942,7.24246834654844,-7.94891084739874));
#16147=CARTESIAN_POINT('Ctrl Pts',(10.0502525316942,7.17831007049655,-7.98717978950973));
#16148=CARTESIAN_POINT('Ctrl Pts',(10.0502525316942,7.08640986444703,-8.03941132011984));
#16149=CARTESIAN_POINT('Ctrl Pts',(10.0502525316942,6.97256625288353,-8.09869101763159));
#16150=CARTESIAN_POINT('Ctrl Pts',(10.0502525316942,6.84473975688511,-8.15552703155277));
#16151=CARTESIAN_POINT('Ctrl Pts',(10.0502525316942,6.73121306554077,-8.19531386354866));
#16152=CARTESIAN_POINT('Ctrl Pts',(10.0502525316942,6.63151085898163,-8.21862212728407));
#16153=CARTESIAN_POINT('Ctrl Pts',(10.0502525316942,6.54471580350543,-8.22655212821855));
#16154=CARTESIAN_POINT('Ctrl Pts',(10.0502525316942,6.46935831372323,-8.22086585997457));
#16155=CARTESIAN_POINT('Ctrl Pts',(10.0502525316942,6.40320361025513,-8.20424193086582));
#16156=CARTESIAN_POINT('Ctrl Pts',(10.0502525316942,6.34348879371403,-8.17999182956336));
#16157=CARTESIAN_POINT('Ctrl Pts',(10.0502525316942,6.28737541479209,-8.15151829405778));
#16158=CARTESIAN_POINT('Ctrl Pts',(10.0502525316942,6.23234494937036,-8.12184190992835));
#16159=CARTESIAN_POINT('Ctrl Pts',(10.0502525316942,6.1765889417745,-8.09313431783932));
#16160=CARTESIAN_POINT('Ctrl Pts',(10.0502525316942,6.11948306053102,-8.06615036325875));
#16161=CARTESIAN_POINT('Ctrl Pts',(10.0502525316942,6.06133545932041,-8.04053373452353));
#16162=CARTESIAN_POINT('Ctrl Pts',(10.0502525316942,6.00299507467204,-8.01529125034138));
#16163=CARTESIAN_POINT('Ctrl Pts',(10.0502525316942,5.94551682580168,-7.98919862941808));
#16164=CARTESIAN_POINT('Ctrl Pts',(10.0502525316942,5.88979801918434,-7.96124121028423));
#16165=CARTESIAN_POINT('Ctrl Pts',(10.0502525316942,5.8362470647093,-7.93101524786534));
#16166=CARTESIAN_POINT('Ctrl Pts',(10.0502525316942,5.78493261248025,-7.89853935606421));
#16167=CARTESIAN_POINT('Ctrl Pts',(10.0502525316942,5.73571509186187,-7.86408741650604));
#16168=CARTESIAN_POINT('Ctrl Pts',(10.0502525316942,5.68837508612421,-7.82802562040593));
#16169=CARTESIAN_POINT('Ctrl Pts',(10.0502525316942,5.64275916621446,-7.79062713132508));
#16170=CARTESIAN_POINT('Ctrl Pts',(10.0502525316942,5.59886036305501,-7.75196943392054));
#16171=CARTESIAN_POINT('Ctrl Pts',(10.0502525316942,5.5567547581677,-7.71201392777609));
#16172=CARTESIAN_POINT('Ctrl Pts',(10.0502525316942,5.51656644870714,-7.67064916836037));
#16173=CARTESIAN_POINT('Ctrl Pts',(10.0502525316942,5.47842458761391,-7.62774439672625));
#16174=CARTESIAN_POINT('Ctrl Pts',(10.0502525316942,5.44241518816367,-7.58320832269043));
#16175=CARTESIAN_POINT('Ctrl Pts',(10.0502525316942,5.4085767049601,-7.5369975221287));
#16176=CARTESIAN_POINT('Ctrl Pts',(10.0502525316942,5.38325149258725,-7.49867649345608));
#16177=CARTESIAN_POINT('Ctrl Pts',(10.0502525316942,5.36523734954954,-7.46917564122634));
#16178=CARTESIAN_POINT('Ctrl Pts',(10.0502525316942,5.35366260632437,-7.44917117889019));
#16179=CARTESIAN_POINT('Ctrl Pts',(10.0502525316942,5.34798390487229,-7.43908464225652));
#16180=CARTESIAN_POINT('',(10.0502525316942,4.34180314898733,-8.06781615908999));
#16181=CARTESIAN_POINT('Origin',(10.0502525316942,0.,0.));
#16182=CARTESIAN_POINT('',(10.0502525316942,4.46902397810654,-9.78902788303806));
#16183=CARTESIAN_POINT('Ctrl Pts',(10.0502525316942,4.34180314898733,-8.06781615908999));
#16184=CARTESIAN_POINT('Ctrl Pts',(10.0502525316942,4.34789619493555,-8.07691891810119));
#16185=CARTESIAN_POINT('Ctrl Pts',(10.0502525316942,4.35989510698125,-8.09522509309135));
#16186=CARTESIAN_POINT('Ctrl Pts',(10.0502525316942,4.37733193665808,-8.1229863261673));
#16187=CARTESIAN_POINT('Ctrl Pts',(10.0502525316942,4.39945592264772,-8.16060634100777));
#16188=CARTESIAN_POINT('Ctrl Pts',(10.0502525316942,4.42521825196284,-8.20864682657585));
#16189=CARTESIAN_POINT('Ctrl Pts',(10.0502525316942,4.44905598790391,-8.25771295042534));
#16190=CARTESIAN_POINT('Ctrl Pts',(10.0502525316942,4.47092121748728,-8.30781651946229));
#16191=CARTESIAN_POINT('Ctrl Pts',(10.0502525316942,4.49074778380617,-8.35896957008516));
#16192=CARTESIAN_POINT('Ctrl Pts',(10.0502525316942,4.50845195831808,-8.41118223898599));
#16193=CARTESIAN_POINT('Ctrl Pts',(10.0502525316942,4.52395547727261,-8.46445618393006));
#16194=CARTESIAN_POINT('Ctrl Pts',(10.0502525316942,4.53720779434568,-8.51877787179233));
#16195=CARTESIAN_POINT('Ctrl Pts',(10.0502525316942,4.54820764638295,-8.5741121935049));
#16196=CARTESIAN_POINT('Ctrl Pts',(10.0502525316942,4.55702950966199,-8.63039414709753));
#16197=CARTESIAN_POINT('Ctrl Pts',(10.0502525316942,4.56383755094179,-8.68752517632497));
#16198=CARTESIAN_POINT('Ctrl Pts',(10.0502525316942,4.56884434816008,-8.7453900186693));
#16199=CARTESIAN_POINT('Ctrl Pts',(10.0502525316942,4.57227742599473,-8.80387069695484));
#16200=CARTESIAN_POINT('Ctrl Pts',(10.0502525316942,4.57434503953799,-8.86286066111437));
#16201=CARTESIAN_POINT('Ctrl Pts',(10.0502525316942,4.57519852862449,-8.92228054501355));
#16202=CARTESIAN_POINT('Ctrl Pts',(10.0502525316942,4.57490858968921,-8.98208782772813));
#16203=CARTESIAN_POINT('Ctrl Pts',(10.0502525316942,4.57349279247872,-9.0422641588092));
#16204=CARTESIAN_POINT('Ctrl Pts',(10.0502525316942,4.57093505021141,-9.10280619261976));
#16205=CARTESIAN_POINT('Ctrl Pts',(10.0502525316942,4.5672074024046,-9.16371548601266));
#16206=CARTESIAN_POINT('Ctrl Pts',(10.0502525316942,4.56229279796226,-9.22498785759991));
#16207=CARTESIAN_POINT('Ctrl Pts',(10.0502525316942,4.55620201600645,-9.28660567396873));
#16208=CARTESIAN_POINT('Ctrl Pts',(10.0502525316942,4.54896317065147,-9.34854353993788));
#16209=CARTESIAN_POINT('Ctrl Pts',(10.0502525316942,4.54061558349964,-9.4107719162247));
#16210=CARTESIAN_POINT('Ctrl Pts',(10.0502525316942,4.53120240639841,-9.47326135298215));
#16211=CARTESIAN_POINT('Ctrl Pts',(10.0502525316942,4.52076380103831,-9.53598658803447));
#16212=CARTESIAN_POINT('Ctrl Pts',(10.0502525316942,4.50933089675096,-9.59893007547295));
#16213=CARTESIAN_POINT('Ctrl Pts',(10.0502525316942,4.4969268049629,-9.6620803346471));
#16214=CARTESIAN_POINT('Ctrl Pts',(10.0502525316942,4.48623896772408,-9.71276073586856));
#16215=CARTESIAN_POINT('Ctrl Pts',(10.0502525316942,4.47779691026848,-9.7508598377266));
#16216=CARTESIAN_POINT('Ctrl Pts',(10.0502525316942,4.47197980068818,-9.77629863524131));
#16217=CARTESIAN_POINT('Ctrl Pts',(10.0502525316942,4.46902397810654,-9.78902788303806));
#16218=CARTESIAN_POINT('',(10.0502525316942,2.78743136471945,-8.7276078365385));
#16219=CARTESIAN_POINT('Ctrl Pts',(10.0502525316942,4.46902397810654,-9.78902788303806));
#16220=CARTESIAN_POINT('Ctrl Pts',(10.0502525316942,4.4316481764287,-9.7979092591739));
#16221=CARTESIAN_POINT('Ctrl Pts',(10.0502525316942,4.35880427644625,-9.81447918831044));
#16222=CARTESIAN_POINT('Ctrl Pts',(10.0502525316942,4.25526155603324,-9.83575560039739));
#16223=CARTESIAN_POINT('Ctrl Pts',(10.0502525316942,4.12867141346466,-9.85695433232581));
#16224=CARTESIAN_POINT('Ctrl Pts',(10.0502525316942,3.98953789729602,-9.87150803413088));
#16225=CARTESIAN_POINT('Ctrl Pts',(10.0502525316942,3.86927279048049,-9.87426588302275));
#16226=CARTESIAN_POINT('Ctrl Pts',(10.0502525316942,3.76724770763979,-9.86562368292838));
#16227=CARTESIAN_POINT('Ctrl Pts',(10.0502525316942,3.68225019949279,-9.84634441482148));
#16228=CARTESIAN_POINT('Ctrl Pts',(10.0502525316942,3.61233812130575,-9.81764970735851));
#16229=CARTESIAN_POINT('Ctrl Pts',(10.0502525316942,3.55455833609672,-9.78139648362373));
#16230=CARTESIAN_POINT('Ctrl Pts',(10.0502525316942,3.50525986412372,-9.73988037363202));
#16231=CARTESIAN_POINT('Ctrl Pts',(10.0502525316942,3.46069167580983,-9.6954604444488));
#16232=CARTESIAN_POINT('Ctrl Pts',(10.0502525316942,3.41752510010333,-9.65023117691875));
#16233=CARTESIAN_POINT('Ctrl Pts',(10.0502525316942,3.37336911957977,-9.60569908050971));
#16234=CARTESIAN_POINT('Ctrl Pts',(10.0502525316942,3.32739669964522,-9.56238912688746));
#16235=CARTESIAN_POINT('Ctrl Pts',(10.0502525316942,3.28001101822472,-9.5200576682471));
#16236=CARTESIAN_POINT('Ctrl Pts',(10.0502525316942,3.23232637183425,-9.47802246886347));
#16237=CARTESIAN_POINT('Ctrl Pts',(10.0502525316942,3.18572437199394,-9.43544515599928));
#16238=CARTESIAN_POINT('Ctrl Pts',(10.0502525316942,3.14137195551156,-9.3916380122022));
#16239=CARTESIAN_POINT('Ctrl Pts',(10.0502525316942,3.09978230736302,-9.34634325868463));
#16240=CARTESIAN_POINT('Ctrl Pts',(10.0502525316942,3.06101496566449,-9.29959981236885));
#16241=CARTESIAN_POINT('Ctrl Pts',(10.0502525316942,3.02485255677714,-9.25162502046097));
#16242=CARTESIAN_POINT('Ctrl Pts',(10.0502525316942,2.99097324368151,-9.20269934800391));
#16243=CARTESIAN_POINT('Ctrl Pts',(10.0502525316942,2.95914669449447,-9.15303517679781));
#16244=CARTESIAN_POINT('Ctrl Pts',(10.0502525316942,2.92934233715353,-9.10270404556727));
#16245=CARTESIAN_POINT('Ctrl Pts',(10.0502525316942,2.9016444576704,-9.05169275361811));
#16246=CARTESIAN_POINT('Ctrl Pts',(10.0502525316942,2.87620551770673,-8.99993365903229));
#16247=CARTESIAN_POINT('Ctrl Pts',(10.0502525316942,2.85318875574511,-8.94734231311461));
#16248=CARTESIAN_POINT('Ctrl Pts',(10.0502525316942,2.83270418548989,-8.89385847330528));
#16249=CARTESIAN_POINT('Ctrl Pts',(10.0502525316942,2.81480179823484,-8.83945272393405));
#16250=CARTESIAN_POINT('Ctrl Pts',(10.0502525316942,2.80255793908285,-8.79518133889446));
#16251=CARTESIAN_POINT('Ctrl Pts',(10.0502525316942,2.7945417356489,-8.76155768480736));
#16252=CARTESIAN_POINT('Ctrl Pts',(10.0502525316942,2.78971521950536,-8.73895551818547));
#16253=CARTESIAN_POINT('Ctrl Pts',(10.0502525316942,2.78743136471945,-8.7276078365385));
#16254=CARTESIAN_POINT('',(10.0502525316942,1.6362078766636,-9.01464008964162));
#16255=CARTESIAN_POINT('Origin',(10.0502525316942,0.,0.));
#16256=CARTESIAN_POINT('',(10.0502525316942,1.22531840158854,-10.6909231138624));
#16257=CARTESIAN_POINT('Ctrl Pts',(10.0502525316942,1.6362078766636,-9.01464008964162));
#16258=CARTESIAN_POINT('Ctrl Pts',(10.0502525316942,1.63918980048658,-9.02518018266099));
#16259=CARTESIAN_POINT('Ctrl Pts',(10.0502525316942,1.64494452480213,-9.04629825740996));
#16260=CARTESIAN_POINT('Ctrl Pts',(10.0502525316942,1.65294924248453,-9.07808903572539));
#16261=CARTESIAN_POINT('Ctrl Pts',(10.0502525316942,1.66236517961207,-9.12070448363665));
#16262=CARTESIAN_POINT('Ctrl Pts',(10.0502525316942,1.67202128432359,-9.17435469805521));
#16263=CARTESIAN_POINT('Ctrl Pts',(10.0502525316942,1.67953005230647,-9.22838562038483));
#16264=CARTESIAN_POINT('Ctrl Pts',(10.0502525316942,1.68484226707077,-9.28279367373423));
#16265=CARTESIAN_POINT('Ctrl Pts',(10.0502525316942,1.68789129020751,-9.33756986179013));
#16266=CARTESIAN_POINT('Ctrl Pts',(10.0502525316942,1.68859435873067,-9.39269795157698));
#16267=CARTESIAN_POINT('Ctrl Pts',(10.0502525316942,1.68687652711276,-9.44815533489435));
#16268=CARTESIAN_POINT('Ctrl Pts',(10.0502525316942,1.68269390490855,-9.50391352130234));
#16269=CARTESIAN_POINT('Ctrl Pts',(10.0502525316942,1.67605614008548,-9.55993872975698));
#16270=CARTESIAN_POINT('Ctrl Pts',(10.0502525316942,1.66705415050613,-9.61619215414635));
#16271=CARTESIAN_POINT('Ctrl Pts',(10.0502525316942,1.65587452359108,-9.67263079222962));
#16272=CARTESIAN_POINT('Ctrl Pts',(10.0502525316942,1.64275505105007,-9.72921071303343));
#16273=CARTESIAN_POINT('Ctrl Pts',(10.0502525316942,1.62794857866286,-9.78589002258816));
#16274=CARTESIAN_POINT('Ctrl Pts',(10.0502525316942,1.6116860945735,-9.84263174012077));
#16275=CARTESIAN_POINT('Ctrl Pts',(10.0502525316942,1.59413605700216,-9.89940715053283));
#16276=CARTESIAN_POINT('Ctrl Pts',(10.0502525316942,1.57537884194225,-9.9561976604221));
#16277=CARTESIAN_POINT('Ctrl Pts',(10.0502525316942,1.55543682981627,-10.0129912468249));
#16278=CARTESIAN_POINT('Ctrl Pts',(10.0502525316942,1.53429575504446,-10.0697797567623));
#16279=CARTESIAN_POINT('Ctrl Pts',(10.0502525316942,1.51192854453357,-10.1265560306252));
#16280=CARTESIAN_POINT('Ctrl Pts',(10.0502525316942,1.48832027384755,-10.1833108225988));
#16281=CARTESIAN_POINT('Ctrl Pts',(10.0502525316942,1.4634866435649,-10.2400306932429));
#16282=CARTESIAN_POINT('Ctrl Pts',(10.0502525316942,1.43746223933981,-10.2967001780439));
#16283=CARTESIAN_POINT('Ctrl Pts',(10.0502525316942,1.41029358637873,-10.353303334518));
#16284=CARTESIAN_POINT('Ctrl Pts',(10.0502525316942,1.38203082503059,-10.4098254888505));
#16285=CARTESIAN_POINT('Ctrl Pts',(10.0502525316942,1.35271995777451,-10.4662550259293));
#16286=CARTESIAN_POINT('Ctrl Pts',(10.0502525316942,1.32239601234813,-10.5225848780961));
#16287=CARTESIAN_POINT('Ctrl Pts',(10.0502525316942,1.29108451674038,-10.5788112684272));
#16288=CARTESIAN_POINT('Ctrl Pts',(10.0502525316942,1.26525867423012,-10.6237084709174));
#16289=CARTESIAN_POINT('Ctrl Pts',(10.0502525316942,1.24545653053149,-10.6573341307832));
#16290=CARTESIAN_POINT('Ctrl Pts',(10.0502525316942,1.23206310981062,-10.6797302792078));
#16291=CARTESIAN_POINT('Ctrl Pts',(10.0502525316942,1.22531840158854,-10.6909231138624));
#16292=CARTESIAN_POINT('',(10.0502525316942,-0.0459743785884374,-9.16181196696065));
#16293=CARTESIAN_POINT('Ctrl Pts',(10.0502525316942,1.22531840158854,-10.6909231138624));
#16294=CARTESIAN_POINT('Ctrl Pts',(10.0502525316942,1.18702740569167,-10.6878200466132));
#16295=CARTESIAN_POINT('Ctrl Pts',(10.0502525316942,1.11262835024222,-10.6810689826619));
#16296=CARTESIAN_POINT('Ctrl Pts',(10.0502525316942,1.00757859836431,-10.6693075927691));
#16297=CARTESIAN_POINT('Ctrl Pts',(10.0502525316942,0.880633449950654,-10.6503502795328));
#16298=CARTESIAN_POINT('Ctrl Pts',(10.0502525316942,0.743812271574574,-10.6211970514875));
#16299=CARTESIAN_POINT('Ctrl Pts',(10.0502525316942,0.628581135879223,-10.5866559598108));
#16300=CARTESIAN_POINT('Ctrl Pts',(10.0502525316942,0.534220102715976,-10.5469092546456));
#16301=CARTESIAN_POINT('Ctrl Pts',(10.0502525316942,0.459340290208065,-10.5023079065862));
#16302=CARTESIAN_POINT('Ctrl Pts',(10.0502525316942,0.401717104935218,-10.4534135977985));
#16303=CARTESIAN_POINT('Ctrl Pts',(10.0502525316942,0.357968125936962,-10.4010797975679));
#16304=CARTESIAN_POINT('Ctrl Pts',(10.0502525316942,0.323911676451424,-10.3463615649927));
#16305=CARTESIAN_POINT('Ctrl Pts',(10.0502525316942,0.295251323542574,-10.2903433742921));
#16306=CARTESIAN_POINT('Ctrl Pts',(10.0502525316942,0.268174082740674,-10.2339885791981));
#16307=CARTESIAN_POINT('Ctrl Pts',(10.0502525316942,0.239940424315883,-10.1779910903389));
#16308=CARTESIAN_POINT('Ctrl Pts',(10.0502525316942,0.209601566462139,-10.1225946176937));
#16309=CARTESIAN_POINT('Ctrl Pts',(10.0502525316942,0.177616245484634,-10.0676920272606));
#16310=CARTESIAN_POINT('Ctrl Pts',(10.0502525316942,0.145255042779229,-10.0129788108676));
#16311=CARTESIAN_POINT('Ctrl Pts',(10.0502525316942,0.114091020408568,-9.95808457009925));
#16312=CARTESIAN_POINT('Ctrl Pts',(10.0502525316942,0.0854465176078889,
-9.90271585009609));
#16313=CARTESIAN_POINT('Ctrl Pts',(10.0502525316942,0.0598892603187484,
-9.84678607154126));
#16314=CARTESIAN_POINT('Ctrl Pts',(10.0502525316942,0.0374638466641554,
-9.79035064491696));
#16315=CARTESIAN_POINT('Ctrl Pts',(10.0502525316942,0.0178963780480492,
-9.73354910755133));
#16316=CARTESIAN_POINT('Ctrl Pts',(10.0502525316942,0.000794100811298054,
-9.67654874444263));
#16317=CARTESIAN_POINT('Ctrl Pts',(10.0502525316942,-0.014127673269992,
-9.61948036621956));
#16318=CARTESIAN_POINT('Ctrl Pts',(10.0502525316942,-0.0269201266367305,
-9.56240256296547));
#16319=CARTESIAN_POINT('Ctrl Pts',(10.0502525316942,-0.0374990192894134,
-9.50532882588415));
#16320=CARTESIAN_POINT('Ctrl Pts',(10.0502525316942,-0.0456984490690192,
-9.44824193693312));
#16321=CARTESIAN_POINT('Ctrl Pts',(10.0502525316942,-0.0513370708710194,
-9.39111202409575));
#16322=CARTESIAN_POINT('Ctrl Pts',(10.0502525316942,-0.0542916394702433,
-9.33391578939727));
#16323=CARTESIAN_POINT('Ctrl Pts',(10.0502525316942,-0.0545055203789832,
-9.27664070503215));
#16324=CARTESIAN_POINT('Ctrl Pts',(10.0502525316942,-0.0524695120683302,
-9.23075255525014));
#16325=CARTESIAN_POINT('Ctrl Pts',(10.0502525316942,-0.0497030940542395,
-9.19629741683749));
#16326=CARTESIAN_POINT('Ctrl Pts',(10.0502525316942,-0.0473089300877004,
-9.17331000347738));
#16327=CARTESIAN_POINT('Ctrl Pts',(10.0502525316942,-0.0459743785884374,
-9.16181196696065));
#16328=CARTESIAN_POINT('',(10.0502525316942,-1.22955082275859,-9.07904823952839));
#16329=CARTESIAN_POINT('Origin',(10.0502525316942,0.,0.));
#16330=CARTESIAN_POINT('',(10.0502525316942,-2.13832987737225,-10.5463163022605));
#16331=CARTESIAN_POINT('Ctrl Pts',(10.0502525316942,-1.22955082275859,-9.07904823952839));
#16332=CARTESIAN_POINT('Ctrl Pts',(10.0502525316942,-1.22997191254093,-9.08999392881405));
#16333=CARTESIAN_POINT('Ctrl Pts',(10.0502525316942,-1.23102468846705,-9.11185671902711));
#16334=CARTESIAN_POINT('Ctrl Pts',(10.0502525316942,-1.23323564031797,-9.14456513970113));
#16335=CARTESIAN_POINT('Ctrl Pts',(10.0502525316942,-1.23744944958329,-9.18800452372235));
#16336=CARTESIAN_POINT('Ctrl Pts',(10.0502525316942,-1.24484477628256,-9.24201281020108));
#16337=CARTESIAN_POINT('Ctrl Pts',(10.0502525316942,-1.2543999867847,-9.29571960787763));
#16338=CARTESIAN_POINT('Ctrl Pts',(10.0502525316942,-1.26616078343298,-9.34910630619445));
#16339=CARTESIAN_POINT('Ctrl Pts',(10.0502525316942,-1.28018776310679,-9.40214375674832));
#16340=CARTESIAN_POINT('Ctrl Pts',(10.0502525316942,-1.29655462181801,-9.45479094589287));
#16341=CARTESIAN_POINT('Ctrl Pts',(10.0502525316942,-1.31532565068075,-9.50700321251013));
#16342=CARTESIAN_POINT('Ctrl Pts',(10.0502525316942,-1.33653378795886,-9.55873989768809));
#16343=CARTESIAN_POINT('Ctrl Pts',(10.0502525316942,-1.36015941897336,-9.60997185513068));
#16344=CARTESIAN_POINT('Ctrl Pts',(10.0502525316942,-1.38610408395052,-9.6606902731969));
#16345=CARTESIAN_POINT('Ctrl Pts',(10.0502525316942,-1.41417703928493,-9.7109119130093));
#16346=CARTESIAN_POINT('Ctrl Pts',(10.0502525316942,-1.44413855620418,-9.76066847540881));
#16347=CARTESIAN_POINT('Ctrl Pts',(10.0502525316942,-1.47573521813323,-9.80999825050556));
#16348=CARTESIAN_POINT('Ctrl Pts',(10.0502525316942,-1.50873591460517,-9.85893744675637));
#16349=CARTESIAN_POINT('Ctrl Pts',(10.0502525316942,-1.54297155887855,-9.90751081093262));
#16350=CARTESIAN_POINT('Ctrl Pts',(10.0502525316942,-1.57835996316383,-9.95572549720588));
#16351=CARTESIAN_POINT('Ctrl Pts',(10.0502525316942,-1.61487612711423,-10.003576986989));
#16352=CARTESIAN_POINT('Ctrl Pts',(10.0502525316942,-1.65253109869336,-10.0510531180319));
#16353=CARTESIAN_POINT('Ctrl Pts',(10.0502525316942,-1.69134841350201,-10.0981387150956));
#16354=CARTESIAN_POINT('Ctrl Pts',(10.0502525316942,-1.73133940840847,-10.1448203729832));
#16355=CARTESIAN_POINT('Ctrl Pts',(10.0502525316942,-1.77248499825981,-10.1910901617733));
#16356=CARTESIAN_POINT('Ctrl Pts',(10.0502525316942,-1.81474751134677,-10.2369440613944));
#16357=CARTESIAN_POINT('Ctrl Pts',(10.0502525316942,-1.85807777307013,-10.2823812867227));
#16358=CARTESIAN_POINT('Ctrl Pts',(10.0502525316942,-1.90242356266618,-10.3274033763511));
#16359=CARTESIAN_POINT('Ctrl Pts',(10.0502525316942,-1.94773753991041,-10.3720134991994));
#16360=CARTESIAN_POINT('Ctrl Pts',(10.0502525316942,-1.99398420741813,-10.4162157576914));
#16361=CARTESIAN_POINT('Ctrl Pts',(10.0502525316942,-2.04113811949547,-10.4600144483414));
#16362=CARTESIAN_POINT('Ctrl Pts',(10.0502525316942,-2.07957395387303,-10.4947336011034));
#16363=CARTESIAN_POINT('Ctrl Pts',(10.0502525316942,-2.10879781201984,-10.5205943051056));
#16364=CARTESIAN_POINT('Ctrl Pts',(10.0502525316942,-2.12845650254365,-10.5377555133892));
#16365=CARTESIAN_POINT('Ctrl Pts',(10.0502525316942,-2.13832987737225,-10.5463163022605));
#16366=CARTESIAN_POINT('',(10.0502525316942,-2.87487982939776,-8.69919410795919));
#16367=CARTESIAN_POINT('Ctrl Pts',(10.0502525316942,-2.13832987737225,-10.5463163022605));
#16368=CARTESIAN_POINT('Ctrl Pts',(10.0502525316942,-2.17378787802072,-10.531532541469));
#16369=CARTESIAN_POINT('Ctrl Pts',(10.0502525316942,-2.24245939102107,-10.5021213256069));
#16370=CARTESIAN_POINT('Ctrl Pts',(10.0502525316942,-2.33873317272541,-10.4584734205235));
#16371=CARTESIAN_POINT('Ctrl Pts',(10.0502525316942,-2.45360705137856,-10.4012157360254));
#16372=CARTESIAN_POINT('Ctrl Pts',(10.0502525316942,-2.57472288173342,-10.3312092992132));
#16373=CARTESIAN_POINT('Ctrl Pts',(10.0502525316942,-2.6736404198842,-10.2627503896831));
#16374=CARTESIAN_POINT('Ctrl Pts',(10.0502525316942,-2.751100687992,-10.1957898638803));
#16375=CARTESIAN_POINT('Ctrl Pts',(10.0502525316942,-2.80853304709422,-10.1302323265723));
#16376=CARTESIAN_POINT('Ctrl Pts',(10.0502525316942,-2.84822678059402,-10.0659245320707));
#16377=CARTESIAN_POINT('Ctrl Pts',(10.0502525316942,-2.8736624985001,-10.0026329523419));
#16378=CARTESIAN_POINT('Ctrl Pts',(10.0502525316942,-2.88914324293729,-9.94006879903196));
#16379=CARTESIAN_POINT('Ctrl Pts',(10.0502525316942,-2.89909028540996,-9.8779357976215));
#16380=CARTESIAN_POINT('Ctrl Pts',(10.0502525316942,-2.90742768231934,-9.81597187495431));
#16381=CARTESIAN_POINT('Ctrl Pts',(10.0502525316942,-2.91697531144329,-9.753990418012));
#16382=CARTESIAN_POINT('Ctrl Pts',(10.0502525316942,-2.92871082842625,-9.69193001905628));
#16383=CARTESIAN_POINT('Ctrl Pts',(10.0502525316942,-2.94216484288864,-9.62983054491074));
#16384=CARTESIAN_POINT('Ctrl Pts',(10.0502525316942,-2.95603486191442,-9.56779502233835));
#16385=CARTESIAN_POINT('Ctrl Pts',(10.0502525316942,-2.96871035517328,-9.50595728442294));
#16386=CARTESIAN_POINT('Ctrl Pts',(10.0502525316942,-2.97884302078014,-9.44444686430419));
#16387=CARTESIAN_POINT('Ctrl Pts',(10.0502525316942,-2.98586616479853,-9.38335685712271));
#16388=CARTESIAN_POINT('Ctrl Pts',(10.0502525316942,-2.98975449467364,-9.32275374295661));
#16389=CARTESIAN_POINT('Ctrl Pts',(10.0502525316942,-2.99081162285579,-9.26268559037018));
#16390=CARTESIAN_POINT('Ctrl Pts',(10.0502525316942,-2.98946277417915,-9.20319012929579));
#16391=CARTESIAN_POINT('Ctrl Pts',(10.0502525316942,-2.9860191259415,-9.144303794535));
#16392=CARTESIAN_POINT('Ctrl Pts',(10.0502525316942,-2.98054746086824,-9.08606649232432));
#16393=CARTESIAN_POINT('Ctrl Pts',(10.0502525316942,-2.97297183097014,-9.02851708515246));
#16394=CARTESIAN_POINT('Ctrl Pts',(10.0502525316942,-2.96312913325008,-8.97169046427448));
#16395=CARTESIAN_POINT('Ctrl Pts',(10.0502525316942,-2.95083766730388,-8.91561425843345));
#16396=CARTESIAN_POINT('Ctrl Pts',(10.0502525316942,-2.93597302048693,-8.86030439480771));
#16397=CARTESIAN_POINT('Ctrl Pts',(10.0502525316942,-2.91847745889582,-8.80576645976534));
#16398=CARTESIAN_POINT('Ctrl Pts',(10.0502525316942,-2.90236088180168,-8.76275339706311));
#16399=CARTESIAN_POINT('Ctrl Pts',(10.0502525316942,-2.88908263860953,-8.7308394833358));
#16400=CARTESIAN_POINT('Ctrl Pts',(10.0502525316942,-2.87970215198308,-8.70971699141988));
#16401=CARTESIAN_POINT('Ctrl Pts',(10.0502525316942,-2.87487982939776,-8.69919410795919));
#16402=CARTESIAN_POINT('',(10.0502525316942,-3.97495252086484,-8.25473589028142));
#16403=CARTESIAN_POINT('Origin',(10.0502525316942,0.,0.));
#16404=CARTESIAN_POINT('',(10.0502525316942,-5.29266352931554,-9.36936257048691));
#16405=CARTESIAN_POINT('Ctrl Pts',(10.0502525316942,-3.97495252086484,-8.25473589028142));
#16406=CARTESIAN_POINT('Ctrl Pts',(10.0502525316942,-3.9787354050507,-8.26501573550299));
#16407=CARTESIAN_POINT('Ctrl Pts',(10.0502525316942,-3.98649262817573,-8.28548315894707));
#16408=CARTESIAN_POINT('Ctrl Pts',(10.0502525316942,-3.9987028261882,-8.31590749387114));
#16409=CARTESIAN_POINT('Ctrl Pts',(10.0502525316942,-4.01613390483614,-8.35591866443433));
#16410=CARTESIAN_POINT('Ctrl Pts',(10.0502525316942,-4.03985675684261,-8.40499831559484));
#16411=CARTESIAN_POINT('Ctrl Pts',(10.0502525316942,-4.06554061525075,-8.45312379306447));
#16412=CARTESIAN_POINT('Ctrl Pts',(10.0502525316942,-4.09322319459339,-8.50026327435046));
#16413=CARTESIAN_POINT('Ctrl Pts',(10.0502525316942,-4.12295311857557,-8.54637031220843));
#16414=CARTESIAN_POINT('Ctrl Pts',(10.0502525316942,-4.1547878023559,-8.59138312702269));
#16415=CARTESIAN_POINT('Ctrl Pts',(10.0502525316942,-4.18877458937294,-8.63523937649908));
#16416=CARTESIAN_POINT('Ctrl Pts',(10.0502525316942,-4.22493224148239,-8.67789021323112));
#16417=CARTESIAN_POINT('Ctrl Pts',(10.0502525316942,-4.26323309731516,-8.71931397871314));
#16418=CARTESIAN_POINT('Ctrl Pts',(10.0502525316942,-4.30358079311506,-8.75953271831989));
#16419=CARTESIAN_POINT('Ctrl Pts',(10.0502525316942,-4.34579910040493,-8.79862131584184));
#16420=CARTESIAN_POINT('Ctrl Pts',(10.0502525316942,-4.38966981967219,-8.83668400083504));
#16421=CARTESIAN_POINT('Ctrl Pts',(10.0502525316942,-4.43496376972658,-8.87383549938658));
#16422=CARTESIAN_POINT('Ctrl Pts',(10.0502525316942,-4.48147234048105,-8.91018166484712));
#16423=CARTESIAN_POINT('Ctrl Pts',(10.0502525316942,-4.52904236806123,-8.94579828347148));
#16424=CARTESIAN_POINT('Ctrl Pts',(10.0502525316942,-4.57759789799493,-8.98071755670482));
#16425=CARTESIAN_POINT('Ctrl Pts',(10.0502525316942,-4.62711375721922,-9.01494291264748));
#16426=CARTESIAN_POINT('Ctrl Pts',(10.0502525316942,-4.67759669462988,-9.04845937030362));
#16427=CARTESIAN_POINT('Ctrl Pts',(10.0502525316942,-4.72906440450668,-9.08124522426278));
#16428=CARTESIAN_POINT('Ctrl Pts',(10.0502525316942,-4.78152352641848,-9.11328422214026));
#16429=CARTESIAN_POINT('Ctrl Pts',(10.0502525316942,-4.83495345882569,-9.14457471976904));
#16430=CARTESIAN_POINT('Ctrl Pts',(10.0502525316942,-4.88931713153333,-9.17512453503235));
#16431=CARTESIAN_POINT('Ctrl Pts',(10.0502525316942,-4.9445675341018,-9.20494811701998));
#16432=CARTESIAN_POINT('Ctrl Pts',(10.0502525316942,-5.00065547708482,-9.23406306612411));
#16433=CARTESIAN_POINT('Ctrl Pts',(10.0502525316942,-5.05753691650348,-9.26248702510056));
#16434=CARTESIAN_POINT('Ctrl Pts',(10.0502525316942,-5.11517936005741,-9.29023486488122));
#16435=CARTESIAN_POINT('Ctrl Pts',(10.0502525316942,-5.17355993514958,-9.31731853484592));
#16436=CARTESIAN_POINT('Ctrl Pts',(10.0502525316942,-5.22084339412737,-9.33846108530483));
#16437=CARTESIAN_POINT('Ctrl Pts',(10.0502525316942,-5.25662833187234,-9.35402540755351));
#16438=CARTESIAN_POINT('Ctrl Pts',(10.0502525316942,-5.28062796260048,-9.3642718170601));
#16439=CARTESIAN_POINT('Ctrl Pts',(10.0502525316942,-5.29266352931554,-9.36936257048691));
#16440=CARTESIAN_POINT('',(10.0502525316942,-5.42237201204004,-7.38503851882133));
#16441=CARTESIAN_POINT('Ctrl Pts',(10.0502525316942,-5.29266352931554,-9.36936257048691));
#16442=CARTESIAN_POINT('Ctrl Pts',(10.0502525316942,-5.32181765856171,-9.34434525366385));
#16443=CARTESIAN_POINT('Ctrl Pts',(10.0502525316942,-5.37803958295792,-9.29515286061949));
#16444=CARTESIAN_POINT('Ctrl Pts',(10.0502525316942,-5.45611344595659,-9.22389100140796));
#16445=CARTESIAN_POINT('Ctrl Pts',(10.0502525316942,-5.54767139923329,-9.13393772674446));
#16446=CARTESIAN_POINT('Ctrl Pts',(10.0502525316942,-5.64122622022819,-9.02993079896417));
#16447=CARTESIAN_POINT('Ctrl Pts',(10.0502525316942,-5.71414742300118,-8.93425530662678));
#16448=CARTESIAN_POINT('Ctrl Pts',(10.0502525316942,-5.76712457531372,-8.84663552299331));
#16449=CARTESIAN_POINT('Ctrl Pts',(10.0502525316942,-5.80148760154654,-8.76653902495464));
#16450=CARTESIAN_POINT('Ctrl Pts',(10.0502525316942,-5.81936638407584,-8.69311263972367));
#16451=CARTESIAN_POINT('Ctrl Pts',(10.0502525316942,-5.82399901560002,-8.62505870129886));
#16452=CARTESIAN_POINT('Ctrl Pts',(10.0502525316942,-5.81938869186267,-8.56077284249031));
#16453=CARTESIAN_POINT('Ctrl Pts',(10.0502525316942,-5.80964873807682,-8.4986070414541));
#16454=CARTESIAN_POINT('Ctrl Pts',(10.0502525316942,-5.79843016859412,-8.43709945169241));
#16455=CARTESIAN_POINT('Ctrl Pts',(10.0502525316942,-5.78835717995633,-8.37520120352267));
#16456=CARTESIAN_POINT('Ctrl Pts',(10.0502525316942,-5.78034060190006,-8.31255178250645));
#16457=CARTESIAN_POINT('Ctrl Pts',(10.0502525316942,-5.77394633717213,-8.24933415385039));
#16458=CARTESIAN_POINT('Ctrl Pts',(10.0502525316942,-5.76796747841793,-8.18604879427487));
#16459=CARTESIAN_POINT('Ctrl Pts',(10.0502525316942,-5.76091367696946,-8.12332066784839));
#16460=CARTESIAN_POINT('Ctrl Pts',(10.0502525316942,-5.75154264947447,-8.06168961610356));
#16461=CARTESIAN_POINT('Ctrl Pts',(10.0502525316942,-5.73934420595248,-8.00141929583747));
#16462=CARTESIAN_POINT('Ctrl Pts',(10.0502525316942,-5.72431483522833,-7.94258074919088));
#16463=CARTESIAN_POINT('Ctrl Pts',(10.0502525316942,-5.70675814390461,-7.88512587067823));
#16464=CARTESIAN_POINT('Ctrl Pts',(10.0502525316942,-5.68709020402104,-7.82895914189736));
#16465=CARTESIAN_POINT('Ctrl Pts',(10.0502525316942,-5.66561822174726,-7.77401905533046));
#16466=CARTESIAN_POINT('Ctrl Pts',(10.0502525316942,-5.64241804293469,-7.72032292706671));
#16467=CARTESIAN_POINT('Ctrl Pts',(10.0502525316942,-5.61742944592276,-7.6679311867486));
#16468=CARTESIAN_POINT('Ctrl Pts',(10.0502525316942,-5.59050809253397,-7.61692741952956));
#16469=CARTESIAN_POINT('Ctrl Pts',(10.0502525316942,-5.56148971316608,-7.56739405041849));
#16470=CARTESIAN_POINT('Ctrl Pts',(10.0502525316942,-5.53026090613148,-7.51938467268366));
#16471=CARTESIAN_POINT('Ctrl Pts',(10.0502525316942,-5.4967684895078,-7.47292244003411));
#16472=CARTESIAN_POINT('Ctrl Pts',(10.0502525316942,-5.46814894648693,-7.43699488267859));
#16473=CARTESIAN_POINT('Ctrl Pts',(10.0502525316942,-5.44565864507534,-7.41074614986957));
#16474=CARTESIAN_POINT('Ctrl Pts',(10.0502525316942,-5.43021006317766,-7.39355619607562));
#16475=CARTESIAN_POINT('Ctrl Pts',(10.0502525316942,-5.42237201204004,-7.38503851882133));
#16476=CARTESIAN_POINT('',(10.0502525316942,-6.33125817110613,-6.62239247796685));
#16477=CARTESIAN_POINT('Origin',(10.0502525316942,0.,0.));
#16478=CARTESIAN_POINT('',(10.0502525316942,-7.92891439885425,-7.2752703501265));
#16479=CARTESIAN_POINT('Ctrl Pts',(10.0502525316942,-6.33125817110613,-6.62239247796685));
#16480=CARTESIAN_POINT('Ctrl Pts',(10.0502525316942,-6.33803255463449,-6.63100021625014));
#16481=CARTESIAN_POINT('Ctrl Pts',(10.0502525316942,-6.35173489391119,-6.64806877891362));
#16482=CARTESIAN_POINT('Ctrl Pts',(10.0502525316942,-6.37274911883029,-6.67323088220656));
#16483=CARTESIAN_POINT('Ctrl Pts',(10.0502525316942,-6.40169119143333,-6.70589726716279));
#16484=CARTESIAN_POINT('Ctrl Pts',(10.0502525316942,-6.43941941070578,-6.74524402479143));
#16485=CARTESIAN_POINT('Ctrl Pts',(10.0502525316942,-6.47871780200897,-6.78307732500951));
#16486=CARTESIAN_POINT('Ctrl Pts',(10.0502525316942,-6.51961240030403,-6.81935524839631));
#16487=CARTESIAN_POINT('Ctrl Pts',(10.0502525316942,-6.56213509649465,-6.85401859544624));
#16488=CARTESIAN_POINT('Ctrl Pts',(10.0502525316942,-6.60632140469039,-6.88699086799345));
#16489=CARTESIAN_POINT('Ctrl Pts',(10.0502525316942,-6.65219708634863,-6.91819814506577));
#16490=CARTESIAN_POINT('Ctrl Pts',(10.0502525316942,-6.69976489037577,-6.9475881722867));
#16491=CARTESIAN_POINT('Ctrl Pts',(10.0502525316942,-6.74899181640015,-6.97514889902642));
#16492=CARTESIAN_POINT('Ctrl Pts',(10.0502525316942,-6.79979302943897,-7.00093106972056));
#16493=CARTESIAN_POINT('Ctrl Pts',(10.0502525316942,-6.85202406661451,-7.02506036068034));
#16494=CARTESIAN_POINT('Ctrl Pts',(10.0502525316942,-6.90550961656264,-7.04770332746178));
#16495=CARTESIAN_POINT('Ctrl Pts',(10.0502525316942,-6.96006716732954,-7.06903990194018));
#16496=CARTESIAN_POINT('Ctrl Pts',(10.0502525316942,-7.01553102941681,-7.08923522069654));
#16497=CARTESIAN_POINT('Ctrl Pts',(10.0502525316942,-7.07177895456439,-7.10840869098247));
#16498=CARTESIAN_POINT('Ctrl Pts',(10.0502525316942,-7.12874865657033,-7.12661440941494));
#16499=CARTESIAN_POINT('Ctrl Pts',(10.0502525316942,-7.18641725377035,-7.14386341521534));
#16500=CARTESIAN_POINT('Ctrl Pts',(10.0502525316942,-7.24478653536347,-7.16013937508649));
#16501=CARTESIAN_POINT('Ctrl Pts',(10.0502525316942,-7.30386662226907,-7.17541617812316));
#16502=CARTESIAN_POINT('Ctrl Pts',(10.0502525316942,-7.36365880682929,-7.18967631564937));
#16503=CARTESIAN_POINT('Ctrl Pts',(10.0502525316942,-7.42414298774012,-7.2029245901952));
#16504=CARTESIAN_POINT('Ctrl Pts',(10.0502525316942,-7.48528632500984,-7.21517989232968));
#16505=CARTESIAN_POINT('Ctrl Pts',(10.0502525316942,-7.54704857406782,-7.22647049097858));
#16506=CARTESIAN_POINT('Ctrl Pts',(10.0502525316942,-7.60938839179095,-7.23682832548438));
#16507=CARTESIAN_POINT('Ctrl Pts',(10.0502525316942,-7.67226934177745,-7.24628378544296));
#16508=CARTESIAN_POINT('Ctrl Pts',(10.0502525316942,-7.73566511738401,-7.254861054624));
#16509=CARTESIAN_POINT('Ctrl Pts',(10.0502525316942,-7.79955765803962,-7.26257856558425));
#16510=CARTESIAN_POINT('Ctrl Pts',(10.0502525316942,-7.85106030720964,-7.26807493359233));
#16511=CARTESIAN_POINT('Ctrl Pts',(10.0502525316942,-7.88990344551799,-7.27181932978281));
#16512=CARTESIAN_POINT('Ctrl Pts',(10.0502525316942,-7.91589476537953,-7.27414795055897));
#16513=CARTESIAN_POINT('Ctrl Pts',(10.0502525316942,-7.92891439885425,-7.2752703501265));
#16514=CARTESIAN_POINT('',(10.0502525316942,-7.43908464225652,-5.34798390487229));
#16515=CARTESIAN_POINT('Ctrl Pts',(10.0502525316942,-7.92891439885425,-7.2752703501265));
#16516=CARTESIAN_POINT('Ctrl Pts',(10.0502525316942,-7.94891084739874,-7.24246834654844));
#16517=CARTESIAN_POINT('Ctrl Pts',(10.0502525316942,-7.98717978950973,-7.17831007049656));
#16518=CARTESIAN_POINT('Ctrl Pts',(10.0502525316942,-8.03941132011984,-7.08640986444703));
#16519=CARTESIAN_POINT('Ctrl Pts',(10.0502525316942,-8.09869101763159,-6.97256625288353));
#16520=CARTESIAN_POINT('Ctrl Pts',(10.0502525316942,-8.15552703155277,-6.84473975688512));
#16521=CARTESIAN_POINT('Ctrl Pts',(10.0502525316942,-8.19531386354866,-6.73121306554078));
#16522=CARTESIAN_POINT('Ctrl Pts',(10.0502525316942,-8.21862212728407,-6.63151085898163));
#16523=CARTESIAN_POINT('Ctrl Pts',(10.0502525316942,-8.22655212821855,-6.54471580350543));
#16524=CARTESIAN_POINT('Ctrl Pts',(10.0502525316942,-8.22086585997457,-6.46935831372324));
#16525=CARTESIAN_POINT('Ctrl Pts',(10.0502525316942,-8.20424193086582,-6.40320361025513));
#16526=CARTESIAN_POINT('Ctrl Pts',(10.0502525316942,-8.17999182956336,-6.34348879371404));
#16527=CARTESIAN_POINT('Ctrl Pts',(10.0502525316942,-8.15151829405778,-6.2873754147921));
#16528=CARTESIAN_POINT('Ctrl Pts',(10.0502525316942,-8.12184190992835,-6.23234494937036));
#16529=CARTESIAN_POINT('Ctrl Pts',(10.0502525316942,-8.09313431783932,-6.1765889417745));
#16530=CARTESIAN_POINT('Ctrl Pts',(10.0502525316942,-8.06615036325875,-6.11948306053102));
#16531=CARTESIAN_POINT('Ctrl Pts',(10.0502525316942,-8.04053373452353,-6.06133545932041));
#16532=CARTESIAN_POINT('Ctrl Pts',(10.0502525316942,-8.01529125034138,-6.00299507467205));
#16533=CARTESIAN_POINT('Ctrl Pts',(10.0502525316942,-7.98919862941808,-5.94551682580168));
#16534=CARTESIAN_POINT('Ctrl Pts',(10.0502525316942,-7.96124121028423,-5.88979801918435));
#16535=CARTESIAN_POINT('Ctrl Pts',(10.0502525316942,-7.93101524786534,-5.83624706470931));
#16536=CARTESIAN_POINT('Ctrl Pts',(10.0502525316942,-7.89853935606421,-5.78493261248025));
#16537=CARTESIAN_POINT('Ctrl Pts',(10.0502525316942,-7.86408741650604,-5.73571509186187));
#16538=CARTESIAN_POINT('Ctrl Pts',(10.0502525316942,-7.82802562040593,-5.68837508612421));
#16539=CARTESIAN_POINT('Ctrl Pts',(10.0502525316942,-7.79062713132508,-5.64275916621446));
#16540=CARTESIAN_POINT('Ctrl Pts',(10.0502525316942,-7.75196943392054,-5.59886036305501));
#16541=CARTESIAN_POINT('Ctrl Pts',(10.0502525316942,-7.71201392777609,-5.55675475816771));
#16542=CARTESIAN_POINT('Ctrl Pts',(10.0502525316942,-7.67064916836037,-5.51656644870715));
#16543=CARTESIAN_POINT('Ctrl Pts',(10.0502525316942,-7.62774439672625,-5.47842458761391));
#16544=CARTESIAN_POINT('Ctrl Pts',(10.0502525316942,-7.58320832269043,-5.44241518816367));
#16545=CARTESIAN_POINT('Ctrl Pts',(10.0502525316942,-7.5369975221287,-5.4085767049601));
#16546=CARTESIAN_POINT('Ctrl Pts',(10.0502525316942,-7.49867649345608,-5.38325149258725));
#16547=CARTESIAN_POINT('Ctrl Pts',(10.0502525316942,-7.46917564122634,-5.36523734954955));
#16548=CARTESIAN_POINT('Ctrl Pts',(10.0502525316942,-7.44917117889019,-5.35366260632437));
#16549=CARTESIAN_POINT('Ctrl Pts',(10.0502525316942,-7.43908464225652,-5.34798390487229));
#16550=CARTESIAN_POINT('',(10.0502525316942,-8.06781615908999,-4.34180314898733));
#16551=CARTESIAN_POINT('Origin',(10.0502525316942,0.,0.));
#16552=CARTESIAN_POINT('',(10.0502525316942,-9.78902788303806,-4.46902397810655));
#16553=CARTESIAN_POINT('Ctrl Pts',(10.0502525316942,-8.06781615908999,-4.34180314898733));
#16554=CARTESIAN_POINT('Ctrl Pts',(10.0502525316942,-8.07691891810119,-4.34789619493555));
#16555=CARTESIAN_POINT('Ctrl Pts',(10.0502525316942,-8.09522509309135,-4.35989510698125));
#16556=CARTESIAN_POINT('Ctrl Pts',(10.0502525316942,-8.1229863261673,-4.37733193665808));
#16557=CARTESIAN_POINT('Ctrl Pts',(10.0502525316942,-8.16060634100777,-4.39945592264773));
#16558=CARTESIAN_POINT('Ctrl Pts',(10.0502525316942,-8.20864682657585,-4.42521825196284));
#16559=CARTESIAN_POINT('Ctrl Pts',(10.0502525316942,-8.25771295042534,-4.44905598790391));
#16560=CARTESIAN_POINT('Ctrl Pts',(10.0502525316942,-8.30781651946229,-4.47092121748728));
#16561=CARTESIAN_POINT('Ctrl Pts',(10.0502525316942,-8.35896957008516,-4.49074778380617));
#16562=CARTESIAN_POINT('Ctrl Pts',(10.0502525316942,-8.41118223898599,-4.50845195831808));
#16563=CARTESIAN_POINT('Ctrl Pts',(10.0502525316942,-8.46445618393006,-4.52395547727261));
#16564=CARTESIAN_POINT('Ctrl Pts',(10.0502525316942,-8.51877787179233,-4.53720779434568));
#16565=CARTESIAN_POINT('Ctrl Pts',(10.0502525316942,-8.5741121935049,-4.54820764638295));
#16566=CARTESIAN_POINT('Ctrl Pts',(10.0502525316942,-8.63039414709753,-4.55702950966199));
#16567=CARTESIAN_POINT('Ctrl Pts',(10.0502525316942,-8.68752517632497,-4.5638375509418));
#16568=CARTESIAN_POINT('Ctrl Pts',(10.0502525316942,-8.7453900186693,-4.56884434816008));
#16569=CARTESIAN_POINT('Ctrl Pts',(10.0502525316942,-8.80387069695484,-4.57227742599473));
#16570=CARTESIAN_POINT('Ctrl Pts',(10.0502525316942,-8.86286066111437,-4.57434503953799));
#16571=CARTESIAN_POINT('Ctrl Pts',(10.0502525316942,-8.92228054501355,-4.57519852862449));
#16572=CARTESIAN_POINT('Ctrl Pts',(10.0502525316942,-8.98208782772813,-4.57490858968921));
#16573=CARTESIAN_POINT('Ctrl Pts',(10.0502525316942,-9.0422641588092,-4.57349279247872));
#16574=CARTESIAN_POINT('Ctrl Pts',(10.0502525316942,-9.10280619261976,-4.57093505021141));
#16575=CARTESIAN_POINT('Ctrl Pts',(10.0502525316942,-9.16371548601266,-4.5672074024046));
#16576=CARTESIAN_POINT('Ctrl Pts',(10.0502525316942,-9.22498785759991,-4.56229279796226));
#16577=CARTESIAN_POINT('Ctrl Pts',(10.0502525316942,-9.28660567396873,-4.55620201600645));
#16578=CARTESIAN_POINT('Ctrl Pts',(10.0502525316942,-9.34854353993788,-4.54896317065147));
#16579=CARTESIAN_POINT('Ctrl Pts',(10.0502525316942,-9.4107719162247,-4.54061558349964));
#16580=CARTESIAN_POINT('Ctrl Pts',(10.0502525316942,-9.47326135298215,-4.53120240639841));
#16581=CARTESIAN_POINT('Ctrl Pts',(10.0502525316942,-9.53598658803447,-4.52076380103831));
#16582=CARTESIAN_POINT('Ctrl Pts',(10.0502525316942,-9.59893007547295,-4.50933089675096));
#16583=CARTESIAN_POINT('Ctrl Pts',(10.0502525316942,-9.6620803346471,-4.4969268049629));
#16584=CARTESIAN_POINT('Ctrl Pts',(10.0502525316942,-9.71276073586856,-4.48623896772408));
#16585=CARTESIAN_POINT('Ctrl Pts',(10.0502525316942,-9.7508598377266,-4.47779691026848));
#16586=CARTESIAN_POINT('Ctrl Pts',(10.0502525316942,-9.77629863524131,-4.47197980068818));
#16587=CARTESIAN_POINT('Ctrl Pts',(10.0502525316942,-9.78902788303806,-4.46902397810655));
#16588=CARTESIAN_POINT('',(10.0502525316942,-8.7276078365385,-2.78743136471945));
#16589=CARTESIAN_POINT('Ctrl Pts',(10.0502525316942,-9.78902788303806,-4.46902397810655));
#16590=CARTESIAN_POINT('Ctrl Pts',(10.0502525316942,-9.7979092591739,-4.4316481764287));
#16591=CARTESIAN_POINT('Ctrl Pts',(10.0502525316942,-9.81447918831044,-4.35880427644625));
#16592=CARTESIAN_POINT('Ctrl Pts',(10.0502525316942,-9.83575560039739,-4.25526155603324));
#16593=CARTESIAN_POINT('Ctrl Pts',(10.0502525316942,-9.85695433232581,-4.12867141346467));
#16594=CARTESIAN_POINT('Ctrl Pts',(10.0502525316942,-9.87150803413088,-3.98953789729602));
#16595=CARTESIAN_POINT('Ctrl Pts',(10.0502525316942,-9.87426588302275,-3.86927279048049));
#16596=CARTESIAN_POINT('Ctrl Pts',(10.0502525316942,-9.86562368292838,-3.76724770763979));
#16597=CARTESIAN_POINT('Ctrl Pts',(10.0502525316942,-9.84634441482148,-3.68225019949279));
#16598=CARTESIAN_POINT('Ctrl Pts',(10.0502525316942,-9.81764970735851,-3.61233812130575));
#16599=CARTESIAN_POINT('Ctrl Pts',(10.0502525316942,-9.78139648362373,-3.55455833609672));
#16600=CARTESIAN_POINT('Ctrl Pts',(10.0502525316942,-9.73988037363202,-3.50525986412372));
#16601=CARTESIAN_POINT('Ctrl Pts',(10.0502525316942,-9.6954604444488,-3.46069167580983));
#16602=CARTESIAN_POINT('Ctrl Pts',(10.0502525316942,-9.65023117691875,-3.41752510010333));
#16603=CARTESIAN_POINT('Ctrl Pts',(10.0502525316942,-9.60569908050971,-3.37336911957978));
#16604=CARTESIAN_POINT('Ctrl Pts',(10.0502525316942,-9.56238912688746,-3.32739669964523));
#16605=CARTESIAN_POINT('Ctrl Pts',(10.0502525316942,-9.5200576682471,-3.28001101822472));
#16606=CARTESIAN_POINT('Ctrl Pts',(10.0502525316942,-9.47802246886347,-3.23232637183425));
#16607=CARTESIAN_POINT('Ctrl Pts',(10.0502525316942,-9.43544515599928,-3.18572437199394));
#16608=CARTESIAN_POINT('Ctrl Pts',(10.0502525316942,-9.3916380122022,-3.14137195551156));
#16609=CARTESIAN_POINT('Ctrl Pts',(10.0502525316942,-9.34634325868463,-3.09978230736302));
#16610=CARTESIAN_POINT('Ctrl Pts',(10.0502525316942,-9.29959981236885,-3.06101496566449));
#16611=CARTESIAN_POINT('Ctrl Pts',(10.0502525316942,-9.25162502046097,-3.02485255677714));
#16612=CARTESIAN_POINT('Ctrl Pts',(10.0502525316942,-9.20269934800391,-2.99097324368151));
#16613=CARTESIAN_POINT('Ctrl Pts',(10.0502525316942,-9.15303517679781,-2.95914669449447));
#16614=CARTESIAN_POINT('Ctrl Pts',(10.0502525316942,-9.10270404556727,-2.92934233715353));
#16615=CARTESIAN_POINT('Ctrl Pts',(10.0502525316942,-9.05169275361811,-2.9016444576704));
#16616=CARTESIAN_POINT('Ctrl Pts',(10.0502525316942,-8.99993365903229,-2.87620551770673));
#16617=CARTESIAN_POINT('Ctrl Pts',(10.0502525316942,-8.94734231311461,-2.85318875574511));
#16618=CARTESIAN_POINT('Ctrl Pts',(10.0502525316942,-8.89385847330528,-2.83270418548989));
#16619=CARTESIAN_POINT('Ctrl Pts',(10.0502525316942,-8.83945272393405,-2.81480179823484));
#16620=CARTESIAN_POINT('Ctrl Pts',(10.0502525316942,-8.79518133889446,-2.80255793908285));
#16621=CARTESIAN_POINT('Ctrl Pts',(10.0502525316942,-8.76155768480736,-2.7945417356489));
#16622=CARTESIAN_POINT('Ctrl Pts',(10.0502525316942,-8.73895551818547,-2.78971521950536));
#16623=CARTESIAN_POINT('Ctrl Pts',(10.0502525316942,-8.7276078365385,-2.78743136471945));
#16624=CARTESIAN_POINT('',(10.0502525316942,-9.01464008964162,-1.6362078766636));
#16625=CARTESIAN_POINT('Origin',(10.0502525316942,0.,0.));
#16626=CARTESIAN_POINT('',(10.0502525316942,-10.6909231138624,-1.22531840158854));
#16627=CARTESIAN_POINT('Ctrl Pts',(10.0502525316942,-9.01464008964162,-1.6362078766636));
#16628=CARTESIAN_POINT('Ctrl Pts',(10.0502525316942,-9.02518018266099,-1.63918980048658));
#16629=CARTESIAN_POINT('Ctrl Pts',(10.0502525316942,-9.04629825740996,-1.64494452480213));
#16630=CARTESIAN_POINT('Ctrl Pts',(10.0502525316942,-9.07808903572539,-1.65294924248453));
#16631=CARTESIAN_POINT('Ctrl Pts',(10.0502525316942,-9.12070448363665,-1.66236517961207));
#16632=CARTESIAN_POINT('Ctrl Pts',(10.0502525316942,-9.17435469805521,-1.67202128432359));
#16633=CARTESIAN_POINT('Ctrl Pts',(10.0502525316942,-9.22838562038483,-1.67953005230647));
#16634=CARTESIAN_POINT('Ctrl Pts',(10.0502525316942,-9.28279367373423,-1.68484226707077));
#16635=CARTESIAN_POINT('Ctrl Pts',(10.0502525316942,-9.33756986179013,-1.68789129020751));
#16636=CARTESIAN_POINT('Ctrl Pts',(10.0502525316942,-9.39269795157698,-1.68859435873067));
#16637=CARTESIAN_POINT('Ctrl Pts',(10.0502525316942,-9.44815533489435,-1.68687652711276));
#16638=CARTESIAN_POINT('Ctrl Pts',(10.0502525316942,-9.50391352130234,-1.68269390490855));
#16639=CARTESIAN_POINT('Ctrl Pts',(10.0502525316942,-9.55993872975698,-1.67605614008548));
#16640=CARTESIAN_POINT('Ctrl Pts',(10.0502525316942,-9.61619215414635,-1.66705415050613));
#16641=CARTESIAN_POINT('Ctrl Pts',(10.0502525316942,-9.67263079222962,-1.65587452359108));
#16642=CARTESIAN_POINT('Ctrl Pts',(10.0502525316942,-9.72921071303343,-1.64275505105007));
#16643=CARTESIAN_POINT('Ctrl Pts',(10.0502525316942,-9.78589002258816,-1.62794857866286));
#16644=CARTESIAN_POINT('Ctrl Pts',(10.0502525316942,-9.84263174012077,-1.6116860945735));
#16645=CARTESIAN_POINT('Ctrl Pts',(10.0502525316942,-9.89940715053283,-1.59413605700216));
#16646=CARTESIAN_POINT('Ctrl Pts',(10.0502525316942,-9.9561976604221,-1.57537884194225));
#16647=CARTESIAN_POINT('Ctrl Pts',(10.0502525316942,-10.0129912468249,-1.55543682981628));
#16648=CARTESIAN_POINT('Ctrl Pts',(10.0502525316942,-10.0697797567623,-1.53429575504446));
#16649=CARTESIAN_POINT('Ctrl Pts',(10.0502525316942,-10.1265560306252,-1.51192854453357));
#16650=CARTESIAN_POINT('Ctrl Pts',(10.0502525316942,-10.1833108225988,-1.48832027384755));
#16651=CARTESIAN_POINT('Ctrl Pts',(10.0502525316942,-10.2400306932429,-1.4634866435649));
#16652=CARTESIAN_POINT('Ctrl Pts',(10.0502525316942,-10.2967001780439,-1.43746223933981));
#16653=CARTESIAN_POINT('Ctrl Pts',(10.0502525316942,-10.353303334518,-1.41029358637873));
#16654=CARTESIAN_POINT('Ctrl Pts',(10.0502525316942,-10.4098254888505,-1.38203082503059));
#16655=CARTESIAN_POINT('Ctrl Pts',(10.0502525316942,-10.4662550259293,-1.35271995777451));
#16656=CARTESIAN_POINT('Ctrl Pts',(10.0502525316942,-10.5225848780961,-1.32239601234813));
#16657=CARTESIAN_POINT('Ctrl Pts',(10.0502525316942,-10.5788112684272,-1.29108451674038));
#16658=CARTESIAN_POINT('Ctrl Pts',(10.0502525316942,-10.6237084709174,-1.26525867423012));
#16659=CARTESIAN_POINT('Ctrl Pts',(10.0502525316942,-10.6573341307832,-1.24545653053149));
#16660=CARTESIAN_POINT('Ctrl Pts',(10.0502525316942,-10.6797302792078,-1.23206310981063));
#16661=CARTESIAN_POINT('Ctrl Pts',(10.0502525316942,-10.6909231138624,-1.22531840158854));
#16662=CARTESIAN_POINT('',(10.0502525316942,-9.16181196696065,0.0459743785884369));
#16663=CARTESIAN_POINT('Ctrl Pts',(10.0502525316942,-10.6909231138624,-1.22531840158854));
#16664=CARTESIAN_POINT('Ctrl Pts',(10.0502525316942,-10.6878200466132,-1.18702740569167));
#16665=CARTESIAN_POINT('Ctrl Pts',(10.0502525316942,-10.6810689826619,-1.11262835024222));
#16666=CARTESIAN_POINT('Ctrl Pts',(10.0502525316942,-10.6693075927691,-1.00757859836431));
#16667=CARTESIAN_POINT('Ctrl Pts',(10.0502525316942,-10.6503502795328,-0.880633449950655));
#16668=CARTESIAN_POINT('Ctrl Pts',(10.0502525316942,-10.6211970514875,-0.743812271574575));
#16669=CARTESIAN_POINT('Ctrl Pts',(10.0502525316942,-10.5866559598108,-0.628581135879224));
#16670=CARTESIAN_POINT('Ctrl Pts',(10.0502525316942,-10.5469092546456,-0.534220102715976));
#16671=CARTESIAN_POINT('Ctrl Pts',(10.0502525316942,-10.5023079065862,-0.459340290208065));
#16672=CARTESIAN_POINT('Ctrl Pts',(10.0502525316942,-10.4534135977985,-0.401717104935219));
#16673=CARTESIAN_POINT('Ctrl Pts',(10.0502525316942,-10.4010797975679,-0.357968125936962));
#16674=CARTESIAN_POINT('Ctrl Pts',(10.0502525316942,-10.3463615649927,-0.323911676451424));
#16675=CARTESIAN_POINT('Ctrl Pts',(10.0502525316942,-10.2903433742921,-0.295251323542575));
#16676=CARTESIAN_POINT('Ctrl Pts',(10.0502525316942,-10.2339885791981,-0.268174082740675));
#16677=CARTESIAN_POINT('Ctrl Pts',(10.0502525316942,-10.1779910903389,-0.239940424315884));
#16678=CARTESIAN_POINT('Ctrl Pts',(10.0502525316942,-10.1225946176937,-0.20960156646214));
#16679=CARTESIAN_POINT('Ctrl Pts',(10.0502525316942,-10.0676920272606,-0.177616245484634));
#16680=CARTESIAN_POINT('Ctrl Pts',(10.0502525316942,-10.0129788108676,-0.14525504277923));
#16681=CARTESIAN_POINT('Ctrl Pts',(10.0502525316942,-9.95808457009925,-0.114091020408568));
#16682=CARTESIAN_POINT('Ctrl Pts',(10.0502525316942,-9.90271585009609,-0.0854465176078895));
#16683=CARTESIAN_POINT('Ctrl Pts',(10.0502525316942,-9.84678607154126,-0.059889260318749));
#16684=CARTESIAN_POINT('Ctrl Pts',(10.0502525316942,-9.79035064491696,-0.037463846664156));
#16685=CARTESIAN_POINT('Ctrl Pts',(10.0502525316942,-9.73354910755133,-0.0178963780480498));
#16686=CARTESIAN_POINT('Ctrl Pts',(10.0502525316942,-9.67654874444263,-0.000794100811298646));
#16687=CARTESIAN_POINT('Ctrl Pts',(10.0502525316942,-9.61948036621956,0.0141276732699914));
#16688=CARTESIAN_POINT('Ctrl Pts',(10.0502525316942,-9.56240256296547,0.0269201266367299));
#16689=CARTESIAN_POINT('Ctrl Pts',(10.0502525316942,-9.50532882588415,0.0374990192894128));
#16690=CARTESIAN_POINT('Ctrl Pts',(10.0502525316942,-9.44824193693312,0.0456984490690186));
#16691=CARTESIAN_POINT('Ctrl Pts',(10.0502525316942,-9.39111202409575,0.0513370708710189));
#16692=CARTESIAN_POINT('Ctrl Pts',(10.0502525316942,-9.33391578939727,0.0542916394702428));
#16693=CARTESIAN_POINT('Ctrl Pts',(10.0502525316942,-9.27664070503215,0.0545055203789827));
#16694=CARTESIAN_POINT('Ctrl Pts',(10.0502525316942,-9.23075255525014,0.0524695120683297));
#16695=CARTESIAN_POINT('Ctrl Pts',(10.0502525316942,-9.19629741683749,0.049703094054239));
#16696=CARTESIAN_POINT('Ctrl Pts',(10.0502525316942,-9.17331000347738,0.0473089300876998));
#16697=CARTESIAN_POINT('Ctrl Pts',(10.0502525316942,-9.16181196696065,0.0459743785884369));
#16698=CARTESIAN_POINT('',(10.0502525316942,-9.07904823952839,1.22955082275859));
#16699=CARTESIAN_POINT('Origin',(10.0502525316942,0.,0.));
#16700=CARTESIAN_POINT('',(10.0502525316942,-10.5463163022605,2.13832987737225));
#16701=CARTESIAN_POINT('Ctrl Pts',(10.0502525316942,-9.07904823952839,1.22955082275859));
#16702=CARTESIAN_POINT('Ctrl Pts',(10.0502525316942,-9.08999392881405,1.22997191254093));
#16703=CARTESIAN_POINT('Ctrl Pts',(10.0502525316942,-9.11185671902711,1.23102468846705));
#16704=CARTESIAN_POINT('Ctrl Pts',(10.0502525316942,-9.14456513970113,1.23323564031797));
#16705=CARTESIAN_POINT('Ctrl Pts',(10.0502525316942,-9.18800452372235,1.23744944958329));
#16706=CARTESIAN_POINT('Ctrl Pts',(10.0502525316942,-9.24201281020108,1.24484477628256));
#16707=CARTESIAN_POINT('Ctrl Pts',(10.0502525316942,-9.29571960787763,1.2543999867847));
#16708=CARTESIAN_POINT('Ctrl Pts',(10.0502525316942,-9.34910630619445,1.26616078343298));
#16709=CARTESIAN_POINT('Ctrl Pts',(10.0502525316942,-9.40214375674832,1.28018776310679));
#16710=CARTESIAN_POINT('Ctrl Pts',(10.0502525316942,-9.45479094589287,1.29655462181801));
#16711=CARTESIAN_POINT('Ctrl Pts',(10.0502525316942,-9.50700321251013,1.31532565068075));
#16712=CARTESIAN_POINT('Ctrl Pts',(10.0502525316942,-9.55873989768809,1.33653378795886));
#16713=CARTESIAN_POINT('Ctrl Pts',(10.0502525316942,-9.60997185513068,1.36015941897336));
#16714=CARTESIAN_POINT('Ctrl Pts',(10.0502525316942,-9.6606902731969,1.38610408395052));
#16715=CARTESIAN_POINT('Ctrl Pts',(10.0502525316942,-9.7109119130093,1.41417703928493));
#16716=CARTESIAN_POINT('Ctrl Pts',(10.0502525316942,-9.76066847540881,1.44413855620418));
#16717=CARTESIAN_POINT('Ctrl Pts',(10.0502525316942,-9.80999825050556,1.47573521813323));
#16718=CARTESIAN_POINT('Ctrl Pts',(10.0502525316942,-9.85893744675637,1.50873591460517));
#16719=CARTESIAN_POINT('Ctrl Pts',(10.0502525316942,-9.90751081093262,1.54297155887855));
#16720=CARTESIAN_POINT('Ctrl Pts',(10.0502525316942,-9.95572549720588,1.57835996316383));
#16721=CARTESIAN_POINT('Ctrl Pts',(10.0502525316942,-10.003576986989,1.61487612711423));
#16722=CARTESIAN_POINT('Ctrl Pts',(10.0502525316942,-10.0510531180319,1.65253109869336));
#16723=CARTESIAN_POINT('Ctrl Pts',(10.0502525316942,-10.0981387150956,1.69134841350201));
#16724=CARTESIAN_POINT('Ctrl Pts',(10.0502525316942,-10.1448203729832,1.73133940840846));
#16725=CARTESIAN_POINT('Ctrl Pts',(10.0502525316942,-10.1910901617733,1.77248499825981));
#16726=CARTESIAN_POINT('Ctrl Pts',(10.0502525316942,-10.2369440613944,1.81474751134677));
#16727=CARTESIAN_POINT('Ctrl Pts',(10.0502525316942,-10.2823812867227,1.85807777307013));
#16728=CARTESIAN_POINT('Ctrl Pts',(10.0502525316942,-10.3274033763511,1.90242356266618));
#16729=CARTESIAN_POINT('Ctrl Pts',(10.0502525316942,-10.3720134991994,1.94773753991041));
#16730=CARTESIAN_POINT('Ctrl Pts',(10.0502525316942,-10.4162157576914,1.99398420741813));
#16731=CARTESIAN_POINT('Ctrl Pts',(10.0502525316942,-10.4600144483414,2.04113811949547));
#16732=CARTESIAN_POINT('Ctrl Pts',(10.0502525316942,-10.4947336011034,2.07957395387303));
#16733=CARTESIAN_POINT('Ctrl Pts',(10.0502525316942,-10.5205943051056,2.10879781201984));
#16734=CARTESIAN_POINT('Ctrl Pts',(10.0502525316942,-10.5377555133892,2.12845650254365));
#16735=CARTESIAN_POINT('Ctrl Pts',(10.0502525316942,-10.5463163022605,2.13832987737225));
#16736=CARTESIAN_POINT('',(10.0502525316942,-8.69919410795919,2.87487982939776));
#16737=CARTESIAN_POINT('Ctrl Pts',(10.0502525316942,-10.5463163022605,2.13832987737225));
#16738=CARTESIAN_POINT('Ctrl Pts',(10.0502525316942,-10.531532541469,2.17378787802072));
#16739=CARTESIAN_POINT('Ctrl Pts',(10.0502525316942,-10.5021213256069,2.24245939102107));
#16740=CARTESIAN_POINT('Ctrl Pts',(10.0502525316942,-10.4584734205235,2.33873317272541));
#16741=CARTESIAN_POINT('Ctrl Pts',(10.0502525316942,-10.4012157360254,2.45360705137856));
#16742=CARTESIAN_POINT('Ctrl Pts',(10.0502525316942,-10.3312092992132,2.57472288173342));
#16743=CARTESIAN_POINT('Ctrl Pts',(10.0502525316942,-10.2627503896831,2.6736404198842));
#16744=CARTESIAN_POINT('Ctrl Pts',(10.0502525316942,-10.1957898638803,2.751100687992));
#16745=CARTESIAN_POINT('Ctrl Pts',(10.0502525316942,-10.1302323265723,2.80853304709422));
#16746=CARTESIAN_POINT('Ctrl Pts',(10.0502525316942,-10.0659245320707,2.84822678059402));
#16747=CARTESIAN_POINT('Ctrl Pts',(10.0502525316942,-10.0026329523419,2.8736624985001));
#16748=CARTESIAN_POINT('Ctrl Pts',(10.0502525316942,-9.94006879903196,2.88914324293729));
#16749=CARTESIAN_POINT('Ctrl Pts',(10.0502525316942,-9.8779357976215,2.89909028540996));
#16750=CARTESIAN_POINT('Ctrl Pts',(10.0502525316942,-9.81597187495431,2.90742768231934));
#16751=CARTESIAN_POINT('Ctrl Pts',(10.0502525316942,-9.753990418012,2.91697531144329));
#16752=CARTESIAN_POINT('Ctrl Pts',(10.0502525316942,-9.69193001905628,2.92871082842625));
#16753=CARTESIAN_POINT('Ctrl Pts',(10.0502525316942,-9.62983054491074,2.94216484288864));
#16754=CARTESIAN_POINT('Ctrl Pts',(10.0502525316942,-9.56779502233835,2.95603486191442));
#16755=CARTESIAN_POINT('Ctrl Pts',(10.0502525316942,-9.50595728442294,2.96871035517328));
#16756=CARTESIAN_POINT('Ctrl Pts',(10.0502525316942,-9.44444686430419,2.97884302078013));
#16757=CARTESIAN_POINT('Ctrl Pts',(10.0502525316942,-9.38335685712271,2.98586616479853));
#16758=CARTESIAN_POINT('Ctrl Pts',(10.0502525316942,-9.32275374295661,2.98975449467364));
#16759=CARTESIAN_POINT('Ctrl Pts',(10.0502525316942,-9.26268559037018,2.99081162285579));
#16760=CARTESIAN_POINT('Ctrl Pts',(10.0502525316942,-9.20319012929579,2.98946277417915));
#16761=CARTESIAN_POINT('Ctrl Pts',(10.0502525316942,-9.144303794535,2.9860191259415));
#16762=CARTESIAN_POINT('Ctrl Pts',(10.0502525316942,-9.08606649232432,2.98054746086824));
#16763=CARTESIAN_POINT('Ctrl Pts',(10.0502525316942,-9.02851708515246,2.97297183097014));
#16764=CARTESIAN_POINT('Ctrl Pts',(10.0502525316942,-8.97169046427448,2.96312913325008));
#16765=CARTESIAN_POINT('Ctrl Pts',(10.0502525316942,-8.91561425843345,2.95083766730388));
#16766=CARTESIAN_POINT('Ctrl Pts',(10.0502525316942,-8.86030439480771,2.93597302048693));
#16767=CARTESIAN_POINT('Ctrl Pts',(10.0502525316942,-8.80576645976534,2.91847745889582));
#16768=CARTESIAN_POINT('Ctrl Pts',(10.0502525316942,-8.76275339706311,2.90236088180168));
#16769=CARTESIAN_POINT('Ctrl Pts',(10.0502525316942,-8.7308394833358,2.88908263860953));
#16770=CARTESIAN_POINT('Ctrl Pts',(10.0502525316942,-8.70971699141988,2.87970215198308));
#16771=CARTESIAN_POINT('Ctrl Pts',(10.0502525316942,-8.69919410795919,2.87487982939776));
#16772=CARTESIAN_POINT('',(10.0502525316942,-8.25473589028142,3.97495252086484));
#16773=CARTESIAN_POINT('Origin',(10.0502525316942,0.,0.));
#16774=CARTESIAN_POINT('',(10.0502525316942,-9.36936257048691,5.29266352931554));
#16775=CARTESIAN_POINT('Ctrl Pts',(10.0502525316942,-8.25473589028142,3.97495252086484));
#16776=CARTESIAN_POINT('Ctrl Pts',(10.0502525316942,-8.26501573550299,3.9787354050507));
#16777=CARTESIAN_POINT('Ctrl Pts',(10.0502525316942,-8.28548315894707,3.98649262817573));
#16778=CARTESIAN_POINT('Ctrl Pts',(10.0502525316942,-8.31590749387114,3.9987028261882));
#16779=CARTESIAN_POINT('Ctrl Pts',(10.0502525316942,-8.35591866443433,4.01613390483614));
#16780=CARTESIAN_POINT('Ctrl Pts',(10.0502525316942,-8.40499831559484,4.03985675684261));
#16781=CARTESIAN_POINT('Ctrl Pts',(10.0502525316942,-8.45312379306447,4.06554061525075));
#16782=CARTESIAN_POINT('Ctrl Pts',(10.0502525316942,-8.50026327435046,4.09322319459339));
#16783=CARTESIAN_POINT('Ctrl Pts',(10.0502525316942,-8.54637031220843,4.12295311857557));
#16784=CARTESIAN_POINT('Ctrl Pts',(10.0502525316942,-8.59138312702269,4.1547878023559));
#16785=CARTESIAN_POINT('Ctrl Pts',(10.0502525316942,-8.63523937649908,4.18877458937294));
#16786=CARTESIAN_POINT('Ctrl Pts',(10.0502525316942,-8.67789021323112,4.22493224148239));
#16787=CARTESIAN_POINT('Ctrl Pts',(10.0502525316942,-8.71931397871314,4.26323309731516));
#16788=CARTESIAN_POINT('Ctrl Pts',(10.0502525316942,-8.75953271831989,4.30358079311506));
#16789=CARTESIAN_POINT('Ctrl Pts',(10.0502525316942,-8.79862131584184,4.34579910040493));
#16790=CARTESIAN_POINT('Ctrl Pts',(10.0502525316942,-8.83668400083504,4.38966981967219));
#16791=CARTESIAN_POINT('Ctrl Pts',(10.0502525316942,-8.87383549938658,4.43496376972658));
#16792=CARTESIAN_POINT('Ctrl Pts',(10.0502525316942,-8.91018166484712,4.48147234048105));
#16793=CARTESIAN_POINT('Ctrl Pts',(10.0502525316942,-8.94579828347148,4.52904236806123));
#16794=CARTESIAN_POINT('Ctrl Pts',(10.0502525316942,-8.98071755670482,4.57759789799493));
#16795=CARTESIAN_POINT('Ctrl Pts',(10.0502525316942,-9.01494291264748,4.62711375721922));
#16796=CARTESIAN_POINT('Ctrl Pts',(10.0502525316942,-9.04845937030362,4.67759669462988));
#16797=CARTESIAN_POINT('Ctrl Pts',(10.0502525316942,-9.08124522426278,4.72906440450668));
#16798=CARTESIAN_POINT('Ctrl Pts',(10.0502525316942,-9.11328422214026,4.78152352641848));
#16799=CARTESIAN_POINT('Ctrl Pts',(10.0502525316942,-9.14457471976904,4.83495345882569));
#16800=CARTESIAN_POINT('Ctrl Pts',(10.0502525316942,-9.17512453503235,4.88931713153333));
#16801=CARTESIAN_POINT('Ctrl Pts',(10.0502525316942,-9.20494811701998,4.9445675341018));
#16802=CARTESIAN_POINT('Ctrl Pts',(10.0502525316942,-9.23406306612411,5.00065547708482));
#16803=CARTESIAN_POINT('Ctrl Pts',(10.0502525316942,-9.26248702510056,5.05753691650348));
#16804=CARTESIAN_POINT('Ctrl Pts',(10.0502525316942,-9.29023486488122,5.11517936005741));
#16805=CARTESIAN_POINT('Ctrl Pts',(10.0502525316942,-9.31731853484592,5.17355993514958));
#16806=CARTESIAN_POINT('Ctrl Pts',(10.0502525316942,-9.33846108530483,5.22084339412737));
#16807=CARTESIAN_POINT('Ctrl Pts',(10.0502525316942,-9.35402540755351,5.25662833187234));
#16808=CARTESIAN_POINT('Ctrl Pts',(10.0502525316942,-9.3642718170601,5.28062796260048));
#16809=CARTESIAN_POINT('Ctrl Pts',(10.0502525316942,-9.36936257048691,5.29266352931554));
#16810=CARTESIAN_POINT('',(10.0502525316942,-7.38503851882133,5.42237201204004));
#16811=CARTESIAN_POINT('Ctrl Pts',(10.0502525316942,-9.36936257048691,5.29266352931554));
#16812=CARTESIAN_POINT('Ctrl Pts',(10.0502525316942,-9.34434525366385,5.32181765856171));
#16813=CARTESIAN_POINT('Ctrl Pts',(10.0502525316942,-9.29515286061949,5.37803958295792));
#16814=CARTESIAN_POINT('Ctrl Pts',(10.0502525316942,-9.22389100140796,5.45611344595659));
#16815=CARTESIAN_POINT('Ctrl Pts',(10.0502525316942,-9.13393772674446,5.54767139923329));
#16816=CARTESIAN_POINT('Ctrl Pts',(10.0502525316942,-9.02993079896417,5.64122622022819));
#16817=CARTESIAN_POINT('Ctrl Pts',(10.0502525316942,-8.93425530662678,5.71414742300118));
#16818=CARTESIAN_POINT('Ctrl Pts',(10.0502525316942,-8.84663552299331,5.76712457531372));
#16819=CARTESIAN_POINT('Ctrl Pts',(10.0502525316942,-8.76653902495464,5.80148760154654));
#16820=CARTESIAN_POINT('Ctrl Pts',(10.0502525316942,-8.69311263972367,5.81936638407584));
#16821=CARTESIAN_POINT('Ctrl Pts',(10.0502525316942,-8.62505870129886,5.82399901560002));
#16822=CARTESIAN_POINT('Ctrl Pts',(10.0502525316942,-8.56077284249031,5.81938869186267));
#16823=CARTESIAN_POINT('Ctrl Pts',(10.0502525316942,-8.4986070414541,5.80964873807682));
#16824=CARTESIAN_POINT('Ctrl Pts',(10.0502525316942,-8.43709945169241,5.79843016859412));
#16825=CARTESIAN_POINT('Ctrl Pts',(10.0502525316942,-8.37520120352267,5.78835717995633));
#16826=CARTESIAN_POINT('Ctrl Pts',(10.0502525316942,-8.31255178250645,5.78034060190006));
#16827=CARTESIAN_POINT('Ctrl Pts',(10.0502525316942,-8.24933415385039,5.77394633717213));
#16828=CARTESIAN_POINT('Ctrl Pts',(10.0502525316942,-8.18604879427487,5.76796747841793));
#16829=CARTESIAN_POINT('Ctrl Pts',(10.0502525316942,-8.12332066784839,5.76091367696946));
#16830=CARTESIAN_POINT('Ctrl Pts',(10.0502525316942,-8.06168961610356,5.75154264947447));
#16831=CARTESIAN_POINT('Ctrl Pts',(10.0502525316942,-8.00141929583747,5.73934420595248));
#16832=CARTESIAN_POINT('Ctrl Pts',(10.0502525316942,-7.94258074919088,5.72431483522833));
#16833=CARTESIAN_POINT('Ctrl Pts',(10.0502525316942,-7.88512587067823,5.70675814390461));
#16834=CARTESIAN_POINT('Ctrl Pts',(10.0502525316942,-7.82895914189736,5.68709020402104));
#16835=CARTESIAN_POINT('Ctrl Pts',(10.0502525316942,-7.77401905533046,5.66561822174726));
#16836=CARTESIAN_POINT('Ctrl Pts',(10.0502525316942,-7.72032292706671,5.64241804293469));
#16837=CARTESIAN_POINT('Ctrl Pts',(10.0502525316942,-7.6679311867486,5.61742944592276));
#16838=CARTESIAN_POINT('Ctrl Pts',(10.0502525316942,-7.61692741952956,5.59050809253397));
#16839=CARTESIAN_POINT('Ctrl Pts',(10.0502525316942,-7.56739405041849,5.56148971316608));
#16840=CARTESIAN_POINT('Ctrl Pts',(10.0502525316942,-7.51938467268366,5.53026090613148));
#16841=CARTESIAN_POINT('Ctrl Pts',(10.0502525316942,-7.47292244003411,5.4967684895078));
#16842=CARTESIAN_POINT('Ctrl Pts',(10.0502525316942,-7.43699488267859,5.46814894648693));
#16843=CARTESIAN_POINT('Ctrl Pts',(10.0502525316942,-7.41074614986957,5.44565864507534));
#16844=CARTESIAN_POINT('Ctrl Pts',(10.0502525316942,-7.39355619607562,5.43021006317766));
#16845=CARTESIAN_POINT('Ctrl Pts',(10.0502525316942,-7.38503851882133,5.42237201204004));
#16846=CARTESIAN_POINT('',(10.0502525316942,-6.62239247796685,6.33125817110613));
#16847=CARTESIAN_POINT('Origin',(10.0502525316942,0.,0.));
#16848=CARTESIAN_POINT('',(10.0502525316942,-7.2752703501265,7.92891439885425));
#16849=CARTESIAN_POINT('Ctrl Pts',(10.0502525316942,-6.62239247796685,6.33125817110613));
#16850=CARTESIAN_POINT('Ctrl Pts',(10.0502525316942,-6.63100021625014,6.33803255463449));
#16851=CARTESIAN_POINT('Ctrl Pts',(10.0502525316942,-6.64806877891362,6.35173489391119));
#16852=CARTESIAN_POINT('Ctrl Pts',(10.0502525316942,-6.67323088220656,6.37274911883029));
#16853=CARTESIAN_POINT('Ctrl Pts',(10.0502525316942,-6.70589726716279,6.40169119143333));
#16854=CARTESIAN_POINT('Ctrl Pts',(10.0502525316942,-6.74524402479143,6.43941941070578));
#16855=CARTESIAN_POINT('Ctrl Pts',(10.0502525316942,-6.78307732500951,6.47871780200897));
#16856=CARTESIAN_POINT('Ctrl Pts',(10.0502525316942,-6.81935524839631,6.51961240030403));
#16857=CARTESIAN_POINT('Ctrl Pts',(10.0502525316942,-6.85401859544624,6.56213509649465));
#16858=CARTESIAN_POINT('Ctrl Pts',(10.0502525316942,-6.88699086799345,6.60632140469039));
#16859=CARTESIAN_POINT('Ctrl Pts',(10.0502525316942,-6.91819814506577,6.65219708634863));
#16860=CARTESIAN_POINT('Ctrl Pts',(10.0502525316942,-6.9475881722867,6.69976489037577));
#16861=CARTESIAN_POINT('Ctrl Pts',(10.0502525316942,-6.97514889902642,6.74899181640015));
#16862=CARTESIAN_POINT('Ctrl Pts',(10.0502525316942,-7.00093106972056,6.79979302943897));
#16863=CARTESIAN_POINT('Ctrl Pts',(10.0502525316942,-7.02506036068034,6.85202406661451));
#16864=CARTESIAN_POINT('Ctrl Pts',(10.0502525316942,-7.04770332746178,6.90550961656264));
#16865=CARTESIAN_POINT('Ctrl Pts',(10.0502525316942,-7.06903990194018,6.96006716732954));
#16866=CARTESIAN_POINT('Ctrl Pts',(10.0502525316942,-7.08923522069654,7.01553102941681));
#16867=CARTESIAN_POINT('Ctrl Pts',(10.0502525316942,-7.10840869098247,7.07177895456439));
#16868=CARTESIAN_POINT('Ctrl Pts',(10.0502525316942,-7.12661440941494,7.12874865657033));
#16869=CARTESIAN_POINT('Ctrl Pts',(10.0502525316942,-7.14386341521534,7.18641725377035));
#16870=CARTESIAN_POINT('Ctrl Pts',(10.0502525316942,-7.16013937508649,7.24478653536347));
#16871=CARTESIAN_POINT('Ctrl Pts',(10.0502525316942,-7.17541617812316,7.30386662226907));
#16872=CARTESIAN_POINT('Ctrl Pts',(10.0502525316942,-7.18967631564937,7.36365880682929));
#16873=CARTESIAN_POINT('Ctrl Pts',(10.0502525316942,-7.2029245901952,7.42414298774012));
#16874=CARTESIAN_POINT('Ctrl Pts',(10.0502525316942,-7.21517989232968,7.48528632500984));
#16875=CARTESIAN_POINT('Ctrl Pts',(10.0502525316942,-7.22647049097858,7.54704857406782));
#16876=CARTESIAN_POINT('Ctrl Pts',(10.0502525316942,-7.23682832548438,7.60938839179095));
#16877=CARTESIAN_POINT('Ctrl Pts',(10.0502525316942,-7.24628378544296,7.67226934177745));
#16878=CARTESIAN_POINT('Ctrl Pts',(10.0502525316942,-7.254861054624,7.73566511738401));
#16879=CARTESIAN_POINT('Ctrl Pts',(10.0502525316942,-7.26257856558425,7.79955765803962));
#16880=CARTESIAN_POINT('Ctrl Pts',(10.0502525316942,-7.26807493359233,7.85106030720964));
#16881=CARTESIAN_POINT('Ctrl Pts',(10.0502525316942,-7.27181932978281,7.88990344551799));
#16882=CARTESIAN_POINT('Ctrl Pts',(10.0502525316942,-7.27414795055897,7.91589476537953));
#16883=CARTESIAN_POINT('Ctrl Pts',(10.0502525316942,-7.2752703501265,7.92891439885425));
#16884=CARTESIAN_POINT('',(10.0502525316942,-5.34798390487229,7.43908464225652));
#16885=CARTESIAN_POINT('Ctrl Pts',(10.0502525316942,-7.2752703501265,7.92891439885425));
#16886=CARTESIAN_POINT('Ctrl Pts',(10.0502525316942,-7.24246834654844,7.94891084739874));
#16887=CARTESIAN_POINT('Ctrl Pts',(10.0502525316942,-7.17831007049656,7.98717978950973));
#16888=CARTESIAN_POINT('Ctrl Pts',(10.0502525316942,-7.08640986444703,8.03941132011984));
#16889=CARTESIAN_POINT('Ctrl Pts',(10.0502525316942,-6.97256625288353,8.09869101763159));
#16890=CARTESIAN_POINT('Ctrl Pts',(10.0502525316942,-6.84473975688512,8.15552703155277));
#16891=CARTESIAN_POINT('Ctrl Pts',(10.0502525316942,-6.73121306554078,8.19531386354866));
#16892=CARTESIAN_POINT('Ctrl Pts',(10.0502525316942,-6.63151085898163,8.21862212728407));
#16893=CARTESIAN_POINT('Ctrl Pts',(10.0502525316942,-6.54471580350543,8.22655212821855));
#16894=CARTESIAN_POINT('Ctrl Pts',(10.0502525316942,-6.46935831372324,8.22086585997457));
#16895=CARTESIAN_POINT('Ctrl Pts',(10.0502525316942,-6.40320361025513,8.20424193086582));
#16896=CARTESIAN_POINT('Ctrl Pts',(10.0502525316942,-6.34348879371404,8.17999182956336));
#16897=CARTESIAN_POINT('Ctrl Pts',(10.0502525316942,-6.2873754147921,8.15151829405778));
#16898=CARTESIAN_POINT('Ctrl Pts',(10.0502525316942,-6.23234494937036,8.12184190992835));
#16899=CARTESIAN_POINT('Ctrl Pts',(10.0502525316942,-6.1765889417745,8.09313431783932));
#16900=CARTESIAN_POINT('Ctrl Pts',(10.0502525316942,-6.11948306053102,8.06615036325875));
#16901=CARTESIAN_POINT('Ctrl Pts',(10.0502525316942,-6.06133545932041,8.04053373452353));
#16902=CARTESIAN_POINT('Ctrl Pts',(10.0502525316942,-6.00299507467205,8.01529125034138));
#16903=CARTESIAN_POINT('Ctrl Pts',(10.0502525316942,-5.94551682580168,7.98919862941808));
#16904=CARTESIAN_POINT('Ctrl Pts',(10.0502525316942,-5.88979801918435,7.96124121028423));
#16905=CARTESIAN_POINT('Ctrl Pts',(10.0502525316942,-5.83624706470931,7.93101524786534));
#16906=CARTESIAN_POINT('Ctrl Pts',(10.0502525316942,-5.78493261248025,7.89853935606421));
#16907=CARTESIAN_POINT('Ctrl Pts',(10.0502525316942,-5.73571509186187,7.86408741650604));
#16908=CARTESIAN_POINT('Ctrl Pts',(10.0502525316942,-5.68837508612421,7.82802562040593));
#16909=CARTESIAN_POINT('Ctrl Pts',(10.0502525316942,-5.64275916621446,7.79062713132508));
#16910=CARTESIAN_POINT('Ctrl Pts',(10.0502525316942,-5.59886036305501,7.75196943392054));
#16911=CARTESIAN_POINT('Ctrl Pts',(10.0502525316942,-5.55675475816771,7.71201392777609));
#16912=CARTESIAN_POINT('Ctrl Pts',(10.0502525316942,-5.51656644870715,7.67064916836037));
#16913=CARTESIAN_POINT('Ctrl Pts',(10.0502525316942,-5.47842458761391,7.62774439672625));
#16914=CARTESIAN_POINT('Ctrl Pts',(10.0502525316942,-5.44241518816367,7.58320832269043));
#16915=CARTESIAN_POINT('Ctrl Pts',(10.0502525316942,-5.4085767049601,7.5369975221287));
#16916=CARTESIAN_POINT('Ctrl Pts',(10.0502525316942,-5.38325149258725,7.49867649345608));
#16917=CARTESIAN_POINT('Ctrl Pts',(10.0502525316942,-5.36523734954955,7.46917564122634));
#16918=CARTESIAN_POINT('Ctrl Pts',(10.0502525316942,-5.35366260632437,7.44917117889019));
#16919=CARTESIAN_POINT('Ctrl Pts',(10.0502525316942,-5.34798390487229,7.43908464225652));
#16920=CARTESIAN_POINT('',(10.0502525316942,-4.34180314898733,8.06781615908999));
#16921=CARTESIAN_POINT('Origin',(10.0502525316942,0.,0.));
#16922=CARTESIAN_POINT('',(10.0502525316942,-4.46902397810655,9.78902788303806));
#16923=CARTESIAN_POINT('Ctrl Pts',(10.0502525316942,-4.34180314898733,8.06781615908999));
#16924=CARTESIAN_POINT('Ctrl Pts',(10.0502525316942,-4.34789619493555,8.07691891810119));
#16925=CARTESIAN_POINT('Ctrl Pts',(10.0502525316942,-4.35989510698125,8.09522509309135));
#16926=CARTESIAN_POINT('Ctrl Pts',(10.0502525316942,-4.37733193665808,8.1229863261673));
#16927=CARTESIAN_POINT('Ctrl Pts',(10.0502525316942,-4.39945592264773,8.16060634100777));
#16928=CARTESIAN_POINT('Ctrl Pts',(10.0502525316942,-4.42521825196285,8.20864682657585));
#16929=CARTESIAN_POINT('Ctrl Pts',(10.0502525316942,-4.44905598790391,8.25771295042534));
#16930=CARTESIAN_POINT('Ctrl Pts',(10.0502525316942,-4.47092121748728,8.30781651946229));
#16931=CARTESIAN_POINT('Ctrl Pts',(10.0502525316942,-4.49074778380617,8.35896957008516));
#16932=CARTESIAN_POINT('Ctrl Pts',(10.0502525316942,-4.50845195831808,8.41118223898599));
#16933=CARTESIAN_POINT('Ctrl Pts',(10.0502525316942,-4.52395547727261,8.46445618393006));
#16934=CARTESIAN_POINT('Ctrl Pts',(10.0502525316942,-4.53720779434568,8.51877787179233));
#16935=CARTESIAN_POINT('Ctrl Pts',(10.0502525316942,-4.54820764638295,8.5741121935049));
#16936=CARTESIAN_POINT('Ctrl Pts',(10.0502525316942,-4.55702950966199,8.63039414709753));
#16937=CARTESIAN_POINT('Ctrl Pts',(10.0502525316942,-4.5638375509418,8.68752517632497));
#16938=CARTESIAN_POINT('Ctrl Pts',(10.0502525316942,-4.56884434816008,8.7453900186693));
#16939=CARTESIAN_POINT('Ctrl Pts',(10.0502525316942,-4.57227742599473,8.80387069695484));
#16940=CARTESIAN_POINT('Ctrl Pts',(10.0502525316942,-4.57434503953799,8.86286066111437));
#16941=CARTESIAN_POINT('Ctrl Pts',(10.0502525316942,-4.57519852862449,8.92228054501355));
#16942=CARTESIAN_POINT('Ctrl Pts',(10.0502525316942,-4.57490858968921,8.98208782772813));
#16943=CARTESIAN_POINT('Ctrl Pts',(10.0502525316942,-4.57349279247872,9.0422641588092));
#16944=CARTESIAN_POINT('Ctrl Pts',(10.0502525316942,-4.57093505021141,9.10280619261976));
#16945=CARTESIAN_POINT('Ctrl Pts',(10.0502525316942,-4.56720740240461,9.16371548601266));
#16946=CARTESIAN_POINT('Ctrl Pts',(10.0502525316942,-4.56229279796226,9.22498785759991));
#16947=CARTESIAN_POINT('Ctrl Pts',(10.0502525316942,-4.55620201600645,9.28660567396873));
#16948=CARTESIAN_POINT('Ctrl Pts',(10.0502525316942,-4.54896317065147,9.34854353993788));
#16949=CARTESIAN_POINT('Ctrl Pts',(10.0502525316942,-4.54061558349964,9.4107719162247));
#16950=CARTESIAN_POINT('Ctrl Pts',(10.0502525316942,-4.53120240639841,9.47326135298215));
#16951=CARTESIAN_POINT('Ctrl Pts',(10.0502525316942,-4.52076380103831,9.53598658803447));
#16952=CARTESIAN_POINT('Ctrl Pts',(10.0502525316942,-4.50933089675096,9.59893007547295));
#16953=CARTESIAN_POINT('Ctrl Pts',(10.0502525316942,-4.4969268049629,9.6620803346471));
#16954=CARTESIAN_POINT('Ctrl Pts',(10.0502525316942,-4.48623896772408,9.71276073586856));
#16955=CARTESIAN_POINT('Ctrl Pts',(10.0502525316942,-4.47779691026848,9.7508598377266));
#16956=CARTESIAN_POINT('Ctrl Pts',(10.0502525316942,-4.47197980068818,9.77629863524131));
#16957=CARTESIAN_POINT('Ctrl Pts',(10.0502525316942,-4.46902397810655,9.78902788303806));
#16958=CARTESIAN_POINT('',(10.0502525316942,-2.78743136471945,8.7276078365385));
#16959=CARTESIAN_POINT('Ctrl Pts',(10.0502525316942,-4.46902397810655,9.78902788303806));
#16960=CARTESIAN_POINT('Ctrl Pts',(10.0502525316942,-4.4316481764287,9.7979092591739));
#16961=CARTESIAN_POINT('Ctrl Pts',(10.0502525316942,-4.35880427644625,9.81447918831044));
#16962=CARTESIAN_POINT('Ctrl Pts',(10.0502525316942,-4.25526155603325,9.83575560039739));
#16963=CARTESIAN_POINT('Ctrl Pts',(10.0502525316942,-4.12867141346467,9.85695433232581));
#16964=CARTESIAN_POINT('Ctrl Pts',(10.0502525316942,-3.98953789729602,9.87150803413088));
#16965=CARTESIAN_POINT('Ctrl Pts',(10.0502525316942,-3.86927279048049,9.87426588302275));
#16966=CARTESIAN_POINT('Ctrl Pts',(10.0502525316942,-3.76724770763979,9.86562368292838));
#16967=CARTESIAN_POINT('Ctrl Pts',(10.0502525316942,-3.68225019949279,9.84634441482148));
#16968=CARTESIAN_POINT('Ctrl Pts',(10.0502525316942,-3.61233812130575,9.81764970735851));
#16969=CARTESIAN_POINT('Ctrl Pts',(10.0502525316942,-3.55455833609672,9.78139648362373));
#16970=CARTESIAN_POINT('Ctrl Pts',(10.0502525316942,-3.50525986412372,9.73988037363202));
#16971=CARTESIAN_POINT('Ctrl Pts',(10.0502525316942,-3.46069167580983,9.6954604444488));
#16972=CARTESIAN_POINT('Ctrl Pts',(10.0502525316942,-3.41752510010333,9.65023117691875));
#16973=CARTESIAN_POINT('Ctrl Pts',(10.0502525316942,-3.37336911957978,9.60569908050971));
#16974=CARTESIAN_POINT('Ctrl Pts',(10.0502525316942,-3.32739669964523,9.56238912688746));
#16975=CARTESIAN_POINT('Ctrl Pts',(10.0502525316942,-3.28001101822472,9.5200576682471));
#16976=CARTESIAN_POINT('Ctrl Pts',(10.0502525316942,-3.23232637183425,9.47802246886347));
#16977=CARTESIAN_POINT('Ctrl Pts',(10.0502525316942,-3.18572437199394,9.43544515599928));
#16978=CARTESIAN_POINT('Ctrl Pts',(10.0502525316942,-3.14137195551156,9.3916380122022));
#16979=CARTESIAN_POINT('Ctrl Pts',(10.0502525316942,-3.09978230736302,9.34634325868463));
#16980=CARTESIAN_POINT('Ctrl Pts',(10.0502525316942,-3.06101496566449,9.29959981236885));
#16981=CARTESIAN_POINT('Ctrl Pts',(10.0502525316942,-3.02485255677714,9.25162502046097));
#16982=CARTESIAN_POINT('Ctrl Pts',(10.0502525316942,-2.99097324368151,9.20269934800391));
#16983=CARTESIAN_POINT('Ctrl Pts',(10.0502525316942,-2.95914669449447,9.15303517679781));
#16984=CARTESIAN_POINT('Ctrl Pts',(10.0502525316942,-2.92934233715353,9.10270404556727));
#16985=CARTESIAN_POINT('Ctrl Pts',(10.0502525316942,-2.9016444576704,9.05169275361811));
#16986=CARTESIAN_POINT('Ctrl Pts',(10.0502525316942,-2.87620551770673,8.99993365903229));
#16987=CARTESIAN_POINT('Ctrl Pts',(10.0502525316942,-2.85318875574511,8.94734231311461));
#16988=CARTESIAN_POINT('Ctrl Pts',(10.0502525316942,-2.83270418548989,8.89385847330528));
#16989=CARTESIAN_POINT('Ctrl Pts',(10.0502525316942,-2.81480179823484,8.83945272393405));
#16990=CARTESIAN_POINT('Ctrl Pts',(10.0502525316942,-2.80255793908285,8.79518133889446));
#16991=CARTESIAN_POINT('Ctrl Pts',(10.0502525316942,-2.7945417356489,8.76155768480736));
#16992=CARTESIAN_POINT('Ctrl Pts',(10.0502525316942,-2.78971521950536,8.73895551818547));
#16993=CARTESIAN_POINT('Ctrl Pts',(10.0502525316942,-2.78743136471945,8.7276078365385));
#16994=CARTESIAN_POINT('',(10.0502525316942,-1.6362078766636,9.01464008964162));
#16995=CARTESIAN_POINT('Origin',(10.0502525316942,0.,0.));
#16996=CARTESIAN_POINT('',(10.0502525316942,-1.22531840158854,10.6909231138624));
#16997=CARTESIAN_POINT('Ctrl Pts',(10.0502525316942,-1.6362078766636,9.01464008964162));
#16998=CARTESIAN_POINT('Ctrl Pts',(10.0502525316942,-1.63918980048658,9.02518018266099));
#16999=CARTESIAN_POINT('Ctrl Pts',(10.0502525316942,-1.64494452480213,9.04629825740996));
#17000=CARTESIAN_POINT('Ctrl Pts',(10.0502525316942,-1.65294924248453,9.07808903572539));
#17001=CARTESIAN_POINT('Ctrl Pts',(10.0502525316942,-1.66236517961207,9.12070448363665));
#17002=CARTESIAN_POINT('Ctrl Pts',(10.0502525316942,-1.67202128432359,9.17435469805521));
#17003=CARTESIAN_POINT('Ctrl Pts',(10.0502525316942,-1.67953005230647,9.22838562038483));
#17004=CARTESIAN_POINT('Ctrl Pts',(10.0502525316942,-1.68484226707077,9.28279367373423));
#17005=CARTESIAN_POINT('Ctrl Pts',(10.0502525316942,-1.68789129020751,9.33756986179013));
#17006=CARTESIAN_POINT('Ctrl Pts',(10.0502525316942,-1.68859435873067,9.39269795157698));
#17007=CARTESIAN_POINT('Ctrl Pts',(10.0502525316942,-1.68687652711276,9.44815533489435));
#17008=CARTESIAN_POINT('Ctrl Pts',(10.0502525316942,-1.68269390490855,9.50391352130234));
#17009=CARTESIAN_POINT('Ctrl Pts',(10.0502525316942,-1.67605614008548,9.55993872975698));
#17010=CARTESIAN_POINT('Ctrl Pts',(10.0502525316942,-1.66705415050613,9.61619215414635));
#17011=CARTESIAN_POINT('Ctrl Pts',(10.0502525316942,-1.65587452359108,9.67263079222962));
#17012=CARTESIAN_POINT('Ctrl Pts',(10.0502525316942,-1.64275505105007,9.72921071303343));
#17013=CARTESIAN_POINT('Ctrl Pts',(10.0502525316942,-1.62794857866286,9.78589002258816));
#17014=CARTESIAN_POINT('Ctrl Pts',(10.0502525316942,-1.6116860945735,9.84263174012077));
#17015=CARTESIAN_POINT('Ctrl Pts',(10.0502525316942,-1.59413605700216,9.89940715053283));
#17016=CARTESIAN_POINT('Ctrl Pts',(10.0502525316942,-1.57537884194225,9.9561976604221));
#17017=CARTESIAN_POINT('Ctrl Pts',(10.0502525316942,-1.55543682981628,10.0129912468249));
#17018=CARTESIAN_POINT('Ctrl Pts',(10.0502525316942,-1.53429575504446,10.0697797567623));
#17019=CARTESIAN_POINT('Ctrl Pts',(10.0502525316942,-1.51192854453357,10.1265560306252));
#17020=CARTESIAN_POINT('Ctrl Pts',(10.0502525316942,-1.48832027384755,10.1833108225988));
#17021=CARTESIAN_POINT('Ctrl Pts',(10.0502525316942,-1.4634866435649,10.2400306932429));
#17022=CARTESIAN_POINT('Ctrl Pts',(10.0502525316942,-1.43746223933981,10.2967001780439));
#17023=CARTESIAN_POINT('Ctrl Pts',(10.0502525316942,-1.41029358637874,10.353303334518));
#17024=CARTESIAN_POINT('Ctrl Pts',(10.0502525316942,-1.38203082503059,10.4098254888505));
#17025=CARTESIAN_POINT('Ctrl Pts',(10.0502525316942,-1.35271995777451,10.4662550259293));
#17026=CARTESIAN_POINT('Ctrl Pts',(10.0502525316942,-1.32239601234813,10.5225848780961));
#17027=CARTESIAN_POINT('Ctrl Pts',(10.0502525316942,-1.29108451674038,10.5788112684272));
#17028=CARTESIAN_POINT('Ctrl Pts',(10.0502525316942,-1.26525867423012,10.6237084709174));
#17029=CARTESIAN_POINT('Ctrl Pts',(10.0502525316942,-1.24545653053149,10.6573341307832));
#17030=CARTESIAN_POINT('Ctrl Pts',(10.0502525316942,-1.23206310981063,10.6797302792078));
#17031=CARTESIAN_POINT('Ctrl Pts',(10.0502525316942,-1.22531840158854,10.6909231138624));
#17032=CARTESIAN_POINT('',(10.0502525316942,0.0459743785884363,9.16181196696065));
#17033=CARTESIAN_POINT('Ctrl Pts',(10.0502525316942,-1.22531840158854,10.6909231138624));
#17034=CARTESIAN_POINT('Ctrl Pts',(10.0502525316942,-1.18702740569167,10.6878200466132));
#17035=CARTESIAN_POINT('Ctrl Pts',(10.0502525316942,-1.11262835024222,10.6810689826619));
#17036=CARTESIAN_POINT('Ctrl Pts',(10.0502525316942,-1.00757859836431,10.6693075927691));
#17037=CARTESIAN_POINT('Ctrl Pts',(10.0502525316942,-0.880633449950656,
10.6503502795328));
#17038=CARTESIAN_POINT('Ctrl Pts',(10.0502525316942,-0.743812271574575,
10.6211970514875));
#17039=CARTESIAN_POINT('Ctrl Pts',(10.0502525316942,-0.628581135879225,
10.5866559598108));
#17040=CARTESIAN_POINT('Ctrl Pts',(10.0502525316942,-0.534220102715977,
10.5469092546456));
#17041=CARTESIAN_POINT('Ctrl Pts',(10.0502525316942,-0.459340290208066,
10.5023079065862));
#17042=CARTESIAN_POINT('Ctrl Pts',(10.0502525316942,-0.40171710493522,10.4534135977985));
#17043=CARTESIAN_POINT('Ctrl Pts',(10.0502525316942,-0.357968125936963,
10.4010797975679));
#17044=CARTESIAN_POINT('Ctrl Pts',(10.0502525316942,-0.323911676451425,
10.3463615649927));
#17045=CARTESIAN_POINT('Ctrl Pts',(10.0502525316942,-0.295251323542575,
10.2903433742921));
#17046=CARTESIAN_POINT('Ctrl Pts',(10.0502525316942,-0.268174082740675,
10.2339885791981));
#17047=CARTESIAN_POINT('Ctrl Pts',(10.0502525316942,-0.239940424315884,
10.1779910903389));
#17048=CARTESIAN_POINT('Ctrl Pts',(10.0502525316942,-0.209601566462141,
10.1225946176937));
#17049=CARTESIAN_POINT('Ctrl Pts',(10.0502525316942,-0.177616245484635,
10.0676920272606));
#17050=CARTESIAN_POINT('Ctrl Pts',(10.0502525316942,-0.145255042779231,
10.0129788108676));
#17051=CARTESIAN_POINT('Ctrl Pts',(10.0502525316942,-0.114091020408569,
9.95808457009925));
#17052=CARTESIAN_POINT('Ctrl Pts',(10.0502525316942,-0.0854465176078901,
9.90271585009609));
#17053=CARTESIAN_POINT('Ctrl Pts',(10.0502525316942,-0.0598892603187496,
9.84678607154126));
#17054=CARTESIAN_POINT('Ctrl Pts',(10.0502525316942,-0.0374638466641566,
9.79035064491696));
#17055=CARTESIAN_POINT('Ctrl Pts',(10.0502525316942,-0.0178963780480504,
9.73354910755133));
#17056=CARTESIAN_POINT('Ctrl Pts',(10.0502525316942,-0.000794100811299239,
9.67654874444263));
#17057=CARTESIAN_POINT('Ctrl Pts',(10.0502525316942,0.0141276732699908,
9.61948036621956));
#17058=CARTESIAN_POINT('Ctrl Pts',(10.0502525316942,0.0269201266367293,
9.56240256296547));
#17059=CARTESIAN_POINT('Ctrl Pts',(10.0502525316942,0.0374990192894122,
9.50532882588415));
#17060=CARTESIAN_POINT('Ctrl Pts',(10.0502525316942,0.045698449069018,9.44824193693312));
#17061=CARTESIAN_POINT('Ctrl Pts',(10.0502525316942,0.0513370708710183,
9.39111202409575));
#17062=CARTESIAN_POINT('Ctrl Pts',(10.0502525316942,0.0542916394702422,
9.33391578939727));
#17063=CARTESIAN_POINT('Ctrl Pts',(10.0502525316942,0.0545055203789821,
9.27664070503215));
#17064=CARTESIAN_POINT('Ctrl Pts',(10.0502525316942,0.0524695120683291,
9.23075255525014));
#17065=CARTESIAN_POINT('Ctrl Pts',(10.0502525316942,0.0497030940542384,
9.19629741683749));
#17066=CARTESIAN_POINT('Ctrl Pts',(10.0502525316942,0.0473089300876993,
9.17331000347738));
#17067=CARTESIAN_POINT('Ctrl Pts',(10.0502525316942,0.0459743785884363,
9.16181196696065));
#17068=CARTESIAN_POINT('',(10.0502525316942,1.22955082275859,9.07904823952839));
#17069=CARTESIAN_POINT('Origin',(10.0502525316942,0.,0.));
#17070=CARTESIAN_POINT('',(10.0502525316942,2.13832987737225,10.5463163022605));
#17071=CARTESIAN_POINT('Ctrl Pts',(10.0502525316942,1.22955082275859,9.07904823952839));
#17072=CARTESIAN_POINT('Ctrl Pts',(10.0502525316942,1.22997191254093,9.08999392881406));
#17073=CARTESIAN_POINT('Ctrl Pts',(10.0502525316942,1.23102468846705,9.11185671902711));
#17074=CARTESIAN_POINT('Ctrl Pts',(10.0502525316942,1.23323564031797,9.14456513970113));
#17075=CARTESIAN_POINT('Ctrl Pts',(10.0502525316942,1.23744944958329,9.18800452372235));
#17076=CARTESIAN_POINT('Ctrl Pts',(10.0502525316942,1.24484477628256,9.24201281020108));
#17077=CARTESIAN_POINT('Ctrl Pts',(10.0502525316942,1.2543999867847,9.29571960787763));
#17078=CARTESIAN_POINT('Ctrl Pts',(10.0502525316942,1.26616078343298,9.34910630619445));
#17079=CARTESIAN_POINT('Ctrl Pts',(10.0502525316942,1.28018776310679,9.40214375674832));
#17080=CARTESIAN_POINT('Ctrl Pts',(10.0502525316942,1.29655462181801,9.45479094589287));
#17081=CARTESIAN_POINT('Ctrl Pts',(10.0502525316942,1.31532565068075,9.50700321251013));
#17082=CARTESIAN_POINT('Ctrl Pts',(10.0502525316942,1.33653378795886,9.55873989768809));
#17083=CARTESIAN_POINT('Ctrl Pts',(10.0502525316942,1.36015941897336,9.60997185513068));
#17084=CARTESIAN_POINT('Ctrl Pts',(10.0502525316942,1.38610408395052,9.6606902731969));
#17085=CARTESIAN_POINT('Ctrl Pts',(10.0502525316942,1.41417703928493,9.7109119130093));
#17086=CARTESIAN_POINT('Ctrl Pts',(10.0502525316942,1.44413855620418,9.76066847540881));
#17087=CARTESIAN_POINT('Ctrl Pts',(10.0502525316942,1.47573521813323,9.80999825050557));
#17088=CARTESIAN_POINT('Ctrl Pts',(10.0502525316942,1.50873591460517,9.85893744675637));
#17089=CARTESIAN_POINT('Ctrl Pts',(10.0502525316942,1.54297155887855,9.90751081093262));
#17090=CARTESIAN_POINT('Ctrl Pts',(10.0502525316942,1.57835996316383,9.95572549720588));
#17091=CARTESIAN_POINT('Ctrl Pts',(10.0502525316942,1.61487612711423,10.003576986989));
#17092=CARTESIAN_POINT('Ctrl Pts',(10.0502525316942,1.65253109869336,10.0510531180319));
#17093=CARTESIAN_POINT('Ctrl Pts',(10.0502525316942,1.69134841350201,10.0981387150956));
#17094=CARTESIAN_POINT('Ctrl Pts',(10.0502525316942,1.73133940840846,10.1448203729832));
#17095=CARTESIAN_POINT('Ctrl Pts',(10.0502525316942,1.77248499825981,10.1910901617733));
#17096=CARTESIAN_POINT('Ctrl Pts',(10.0502525316942,1.81474751134677,10.2369440613944));
#17097=CARTESIAN_POINT('Ctrl Pts',(10.0502525316942,1.85807777307013,10.2823812867227));
#17098=CARTESIAN_POINT('Ctrl Pts',(10.0502525316942,1.90242356266618,10.3274033763511));
#17099=CARTESIAN_POINT('Ctrl Pts',(10.0502525316942,1.94773753991041,10.3720134991994));
#17100=CARTESIAN_POINT('Ctrl Pts',(10.0502525316942,1.99398420741813,10.4162157576914));
#17101=CARTESIAN_POINT('Ctrl Pts',(10.0502525316942,2.04113811949547,10.4600144483414));
#17102=CARTESIAN_POINT('Ctrl Pts',(10.0502525316942,2.07957395387303,10.4947336011034));
#17103=CARTESIAN_POINT('Ctrl Pts',(10.0502525316942,2.10879781201984,10.5205943051056));
#17104=CARTESIAN_POINT('Ctrl Pts',(10.0502525316942,2.12845650254365,10.5377555133892));
#17105=CARTESIAN_POINT('Ctrl Pts',(10.0502525316942,2.13832987737225,10.5463163022605));
#17106=CARTESIAN_POINT('',(10.0502525316942,2.87487982939776,8.69919410795919));
#17107=CARTESIAN_POINT('Ctrl Pts',(10.0502525316942,2.13832987737225,10.5463163022605));
#17108=CARTESIAN_POINT('Ctrl Pts',(10.0502525316942,2.17378787802072,10.531532541469));
#17109=CARTESIAN_POINT('Ctrl Pts',(10.0502525316942,2.24245939102107,10.5021213256069));
#17110=CARTESIAN_POINT('Ctrl Pts',(10.0502525316942,2.33873317272541,10.4584734205235));
#17111=CARTESIAN_POINT('Ctrl Pts',(10.0502525316942,2.45360705137856,10.4012157360254));
#17112=CARTESIAN_POINT('Ctrl Pts',(10.0502525316942,2.57472288173342,10.3312092992132));
#17113=CARTESIAN_POINT('Ctrl Pts',(10.0502525316942,2.6736404198842,10.2627503896831));
#17114=CARTESIAN_POINT('Ctrl Pts',(10.0502525316942,2.751100687992,10.1957898638803));
#17115=CARTESIAN_POINT('Ctrl Pts',(10.0502525316942,2.80853304709422,10.1302323265723));
#17116=CARTESIAN_POINT('Ctrl Pts',(10.0502525316942,2.84822678059402,10.0659245320707));
#17117=CARTESIAN_POINT('Ctrl Pts',(10.0502525316942,2.8736624985001,10.0026329523419));
#17118=CARTESIAN_POINT('Ctrl Pts',(10.0502525316942,2.88914324293729,9.94006879903196));
#17119=CARTESIAN_POINT('Ctrl Pts',(10.0502525316942,2.89909028540996,9.8779357976215));
#17120=CARTESIAN_POINT('Ctrl Pts',(10.0502525316942,2.90742768231934,9.81597187495431));
#17121=CARTESIAN_POINT('Ctrl Pts',(10.0502525316942,2.91697531144329,9.753990418012));
#17122=CARTESIAN_POINT('Ctrl Pts',(10.0502525316942,2.92871082842625,9.69193001905628));
#17123=CARTESIAN_POINT('Ctrl Pts',(10.0502525316942,2.94216484288864,9.62983054491075));
#17124=CARTESIAN_POINT('Ctrl Pts',(10.0502525316942,2.95603486191442,9.56779502233836));
#17125=CARTESIAN_POINT('Ctrl Pts',(10.0502525316942,2.96871035517328,9.50595728442294));
#17126=CARTESIAN_POINT('Ctrl Pts',(10.0502525316942,2.97884302078013,9.44444686430419));
#17127=CARTESIAN_POINT('Ctrl Pts',(10.0502525316942,2.98586616479853,9.38335685712271));
#17128=CARTESIAN_POINT('Ctrl Pts',(10.0502525316942,2.98975449467364,9.32275374295661));
#17129=CARTESIAN_POINT('Ctrl Pts',(10.0502525316942,2.99081162285579,9.26268559037018));
#17130=CARTESIAN_POINT('Ctrl Pts',(10.0502525316942,2.98946277417915,9.20319012929579));
#17131=CARTESIAN_POINT('Ctrl Pts',(10.0502525316942,2.9860191259415,9.144303794535));
#17132=CARTESIAN_POINT('Ctrl Pts',(10.0502525316942,2.98054746086824,9.08606649232432));
#17133=CARTESIAN_POINT('Ctrl Pts',(10.0502525316942,2.97297183097014,9.02851708515246));
#17134=CARTESIAN_POINT('Ctrl Pts',(10.0502525316942,2.96312913325008,8.97169046427448));
#17135=CARTESIAN_POINT('Ctrl Pts',(10.0502525316942,2.95083766730388,8.91561425843345));
#17136=CARTESIAN_POINT('Ctrl Pts',(10.0502525316942,2.93597302048693,8.86030439480771));
#17137=CARTESIAN_POINT('Ctrl Pts',(10.0502525316942,2.91847745889582,8.80576645976534));
#17138=CARTESIAN_POINT('Ctrl Pts',(10.0502525316942,2.90236088180168,8.76275339706311));
#17139=CARTESIAN_POINT('Ctrl Pts',(10.0502525316942,2.88908263860953,8.7308394833358));
#17140=CARTESIAN_POINT('Ctrl Pts',(10.0502525316942,2.87970215198308,8.70971699141988));
#17141=CARTESIAN_POINT('Ctrl Pts',(10.0502525316942,2.87487982939776,8.69919410795919));
#17142=CARTESIAN_POINT('',(10.0502525316942,3.97495252086484,8.25473589028142));
#17143=CARTESIAN_POINT('Origin',(10.0502525316942,0.,0.));
#17144=CARTESIAN_POINT('',(10.0502525316942,5.29266352931554,9.36936257048691));
#17145=CARTESIAN_POINT('Ctrl Pts',(10.0502525316942,3.97495252086484,8.25473589028142));
#17146=CARTESIAN_POINT('Ctrl Pts',(10.0502525316942,3.9787354050507,8.26501573550299));
#17147=CARTESIAN_POINT('Ctrl Pts',(10.0502525316942,3.98649262817573,8.28548315894707));
#17148=CARTESIAN_POINT('Ctrl Pts',(10.0502525316942,3.9987028261882,8.31590749387114));
#17149=CARTESIAN_POINT('Ctrl Pts',(10.0502525316942,4.01613390483614,8.35591866443433));
#17150=CARTESIAN_POINT('Ctrl Pts',(10.0502525316942,4.03985675684261,8.40499831559484));
#17151=CARTESIAN_POINT('Ctrl Pts',(10.0502525316942,4.06554061525075,8.45312379306447));
#17152=CARTESIAN_POINT('Ctrl Pts',(10.0502525316942,4.09322319459338,8.50026327435046));
#17153=CARTESIAN_POINT('Ctrl Pts',(10.0502525316942,4.12295311857557,8.54637031220843));
#17154=CARTESIAN_POINT('Ctrl Pts',(10.0502525316942,4.1547878023559,8.59138312702269));
#17155=CARTESIAN_POINT('Ctrl Pts',(10.0502525316942,4.18877458937293,8.63523937649908));
#17156=CARTESIAN_POINT('Ctrl Pts',(10.0502525316942,4.22493224148239,8.67789021323112));
#17157=CARTESIAN_POINT('Ctrl Pts',(10.0502525316942,4.26323309731516,8.71931397871314));
#17158=CARTESIAN_POINT('Ctrl Pts',(10.0502525316942,4.30358079311506,8.75953271831989));
#17159=CARTESIAN_POINT('Ctrl Pts',(10.0502525316942,4.34579910040492,8.79862131584184));
#17160=CARTESIAN_POINT('Ctrl Pts',(10.0502525316942,4.38966981967219,8.83668400083504));
#17161=CARTESIAN_POINT('Ctrl Pts',(10.0502525316942,4.43496376972658,8.87383549938659));
#17162=CARTESIAN_POINT('Ctrl Pts',(10.0502525316942,4.48147234048104,8.91018166484712));
#17163=CARTESIAN_POINT('Ctrl Pts',(10.0502525316942,4.52904236806123,8.94579828347148));
#17164=CARTESIAN_POINT('Ctrl Pts',(10.0502525316942,4.57759789799493,8.98071755670482));
#17165=CARTESIAN_POINT('Ctrl Pts',(10.0502525316942,4.62711375721922,9.01494291264748));
#17166=CARTESIAN_POINT('Ctrl Pts',(10.0502525316942,4.67759669462988,9.04845937030362));
#17167=CARTESIAN_POINT('Ctrl Pts',(10.0502525316942,4.72906440450668,9.08124522426278));
#17168=CARTESIAN_POINT('Ctrl Pts',(10.0502525316942,4.78152352641848,9.11328422214026));
#17169=CARTESIAN_POINT('Ctrl Pts',(10.0502525316942,4.83495345882569,9.14457471976904));
#17170=CARTESIAN_POINT('Ctrl Pts',(10.0502525316942,4.88931713153333,9.17512453503235));
#17171=CARTESIAN_POINT('Ctrl Pts',(10.0502525316942,4.94456753410179,9.20494811701998));
#17172=CARTESIAN_POINT('Ctrl Pts',(10.0502525316942,5.00065547708482,9.23406306612412));
#17173=CARTESIAN_POINT('Ctrl Pts',(10.0502525316942,5.05753691650348,9.26248702510056));
#17174=CARTESIAN_POINT('Ctrl Pts',(10.0502525316942,5.11517936005741,9.29023486488122));
#17175=CARTESIAN_POINT('Ctrl Pts',(10.0502525316942,5.17355993514958,9.31731853484592));
#17176=CARTESIAN_POINT('Ctrl Pts',(10.0502525316942,5.22084339412736,9.33846108530483));
#17177=CARTESIAN_POINT('Ctrl Pts',(10.0502525316942,5.25662833187234,9.35402540755351));
#17178=CARTESIAN_POINT('Ctrl Pts',(10.0502525316942,5.28062796260048,9.3642718170601));
#17179=CARTESIAN_POINT('Ctrl Pts',(10.0502525316942,5.29266352931554,9.36936257048691));
#17180=CARTESIAN_POINT('',(10.0502525316942,5.42237201204004,7.38503851882133));
#17181=CARTESIAN_POINT('Ctrl Pts',(10.0502525316942,5.29266352931554,9.36936257048691));
#17182=CARTESIAN_POINT('Ctrl Pts',(10.0502525316942,5.32181765856171,9.34434525366385));
#17183=CARTESIAN_POINT('Ctrl Pts',(10.0502525316942,5.37803958295792,9.29515286061949));
#17184=CARTESIAN_POINT('Ctrl Pts',(10.0502525316942,5.45611344595659,9.22389100140797));
#17185=CARTESIAN_POINT('Ctrl Pts',(10.0502525316942,5.54767139923329,9.13393772674446));
#17186=CARTESIAN_POINT('Ctrl Pts',(10.0502525316942,5.64122622022818,9.02993079896417));
#17187=CARTESIAN_POINT('Ctrl Pts',(10.0502525316942,5.71414742300118,8.93425530662678));
#17188=CARTESIAN_POINT('Ctrl Pts',(10.0502525316942,5.76712457531372,8.84663552299331));
#17189=CARTESIAN_POINT('Ctrl Pts',(10.0502525316942,5.80148760154654,8.76653902495464));
#17190=CARTESIAN_POINT('Ctrl Pts',(10.0502525316942,5.81936638407584,8.69311263972367));
#17191=CARTESIAN_POINT('Ctrl Pts',(10.0502525316942,5.82399901560002,8.62505870129887));
#17192=CARTESIAN_POINT('Ctrl Pts',(10.0502525316942,5.81938869186267,8.56077284249031));
#17193=CARTESIAN_POINT('Ctrl Pts',(10.0502525316942,5.80964873807682,8.4986070414541));
#17194=CARTESIAN_POINT('Ctrl Pts',(10.0502525316942,5.79843016859412,8.43709945169241));
#17195=CARTESIAN_POINT('Ctrl Pts',(10.0502525316942,5.78835717995633,8.37520120352267));
#17196=CARTESIAN_POINT('Ctrl Pts',(10.0502525316942,5.78034060190006,8.31255178250645));
#17197=CARTESIAN_POINT('Ctrl Pts',(10.0502525316942,5.77394633717213,8.24933415385039));
#17198=CARTESIAN_POINT('Ctrl Pts',(10.0502525316942,5.76796747841793,8.18604879427487));
#17199=CARTESIAN_POINT('Ctrl Pts',(10.0502525316942,5.76091367696946,8.12332066784839));
#17200=CARTESIAN_POINT('Ctrl Pts',(10.0502525316942,5.75154264947446,8.06168961610356));
#17201=CARTESIAN_POINT('Ctrl Pts',(10.0502525316942,5.73934420595248,8.00141929583747));
#17202=CARTESIAN_POINT('Ctrl Pts',(10.0502525316942,5.72431483522833,7.94258074919088));
#17203=CARTESIAN_POINT('Ctrl Pts',(10.0502525316942,5.7067581439046,7.88512587067823));
#17204=CARTESIAN_POINT('Ctrl Pts',(10.0502525316942,5.68709020402104,7.82895914189736));
#17205=CARTESIAN_POINT('Ctrl Pts',(10.0502525316942,5.66561822174726,7.77401905533046));
#17206=CARTESIAN_POINT('Ctrl Pts',(10.0502525316942,5.64241804293469,7.72032292706671));
#17207=CARTESIAN_POINT('Ctrl Pts',(10.0502525316942,5.61742944592276,7.6679311867486));
#17208=CARTESIAN_POINT('Ctrl Pts',(10.0502525316942,5.59050809253397,7.61692741952956));
#17209=CARTESIAN_POINT('Ctrl Pts',(10.0502525316942,5.56148971316608,7.56739405041849));
#17210=CARTESIAN_POINT('Ctrl Pts',(10.0502525316942,5.53026090613148,7.51938467268366));
#17211=CARTESIAN_POINT('Ctrl Pts',(10.0502525316942,5.4967684895078,7.47292244003411));
#17212=CARTESIAN_POINT('Ctrl Pts',(10.0502525316942,5.46814894648693,7.43699488267859));
#17213=CARTESIAN_POINT('Ctrl Pts',(10.0502525316942,5.44565864507534,7.41074614986957));
#17214=CARTESIAN_POINT('Ctrl Pts',(10.0502525316942,5.43021006317766,7.39355619607562));
#17215=CARTESIAN_POINT('Ctrl Pts',(10.0502525316942,5.42237201204004,7.38503851882133));
#17216=CARTESIAN_POINT('',(10.0502525316942,6.33125817110613,6.62239247796685));
#17217=CARTESIAN_POINT('Origin',(10.0502525316942,0.,0.));
#17218=CARTESIAN_POINT('',(10.0502525316942,7.92891439885425,7.2752703501265));
#17219=CARTESIAN_POINT('Ctrl Pts',(10.0502525316942,6.33125817110613,6.62239247796685));
#17220=CARTESIAN_POINT('Ctrl Pts',(10.0502525316942,6.33803255463449,6.63100021625014));
#17221=CARTESIAN_POINT('Ctrl Pts',(10.0502525316942,6.35173489391119,6.64806877891362));
#17222=CARTESIAN_POINT('Ctrl Pts',(10.0502525316942,6.37274911883029,6.67323088220656));
#17223=CARTESIAN_POINT('Ctrl Pts',(10.0502525316942,6.40169119143333,6.70589726716278));
#17224=CARTESIAN_POINT('Ctrl Pts',(10.0502525316942,6.43941941070578,6.74524402479143));
#17225=CARTESIAN_POINT('Ctrl Pts',(10.0502525316942,6.47871780200897,6.7830773250095));
#17226=CARTESIAN_POINT('Ctrl Pts',(10.0502525316942,6.51961240030403,6.81935524839631));
#17227=CARTESIAN_POINT('Ctrl Pts',(10.0502525316942,6.56213509649465,6.85401859544624));
#17228=CARTESIAN_POINT('Ctrl Pts',(10.0502525316942,6.60632140469038,6.88699086799345));
#17229=CARTESIAN_POINT('Ctrl Pts',(10.0502525316942,6.65219708634863,6.91819814506577));
#17230=CARTESIAN_POINT('Ctrl Pts',(10.0502525316942,6.69976489037577,6.9475881722867));
#17231=CARTESIAN_POINT('Ctrl Pts',(10.0502525316942,6.74899181640015,6.97514889902642));
#17232=CARTESIAN_POINT('Ctrl Pts',(10.0502525316942,6.79979302943897,7.00093106972056));
#17233=CARTESIAN_POINT('Ctrl Pts',(10.0502525316942,6.85202406661451,7.02506036068034));
#17234=CARTESIAN_POINT('Ctrl Pts',(10.0502525316942,6.90550961656264,7.04770332746178));
#17235=CARTESIAN_POINT('Ctrl Pts',(10.0502525316942,6.96006716732954,7.06903990194018));
#17236=CARTESIAN_POINT('Ctrl Pts',(10.0502525316942,7.01553102941681,7.08923522069654));
#17237=CARTESIAN_POINT('Ctrl Pts',(10.0502525316942,7.07177895456438,7.10840869098247));
#17238=CARTESIAN_POINT('Ctrl Pts',(10.0502525316942,7.12874865657033,7.12661440941494));
#17239=CARTESIAN_POINT('Ctrl Pts',(10.0502525316942,7.18641725377035,7.14386341521534));
#17240=CARTESIAN_POINT('Ctrl Pts',(10.0502525316942,7.24478653536347,7.16013937508649));
#17241=CARTESIAN_POINT('Ctrl Pts',(10.0502525316942,7.30386662226907,7.17541617812316));
#17242=CARTESIAN_POINT('Ctrl Pts',(10.0502525316942,7.36365880682929,7.18967631564937));
#17243=CARTESIAN_POINT('Ctrl Pts',(10.0502525316942,7.42414298774012,7.2029245901952));
#17244=CARTESIAN_POINT('Ctrl Pts',(10.0502525316942,7.48528632500984,7.21517989232968));
#17245=CARTESIAN_POINT('Ctrl Pts',(10.0502525316942,7.54704857406782,7.22647049097858));
#17246=CARTESIAN_POINT('Ctrl Pts',(10.0502525316942,7.60938839179095,7.23682832548438));
#17247=CARTESIAN_POINT('Ctrl Pts',(10.0502525316942,7.67226934177745,7.24628378544296));
#17248=CARTESIAN_POINT('Ctrl Pts',(10.0502525316942,7.73566511738401,7.254861054624));
#17249=CARTESIAN_POINT('Ctrl Pts',(10.0502525316942,7.79955765803962,7.26257856558425));
#17250=CARTESIAN_POINT('Ctrl Pts',(10.0502525316942,7.85106030720964,7.26807493359233));
#17251=CARTESIAN_POINT('Ctrl Pts',(10.0502525316942,7.88990344551799,7.27181932978281));
#17252=CARTESIAN_POINT('Ctrl Pts',(10.0502525316942,7.91589476537953,7.27414795055897));
#17253=CARTESIAN_POINT('Ctrl Pts',(10.0502525316942,7.92891439885425,7.2752703501265));
#17254=CARTESIAN_POINT('',(10.0502525316942,7.43908464225652,5.34798390487229));
#17255=CARTESIAN_POINT('Ctrl Pts',(10.0502525316942,7.92891439885425,7.2752703501265));
#17256=CARTESIAN_POINT('Ctrl Pts',(10.0502525316942,7.94891084739874,7.24246834654844));
#17257=CARTESIAN_POINT('Ctrl Pts',(10.0502525316942,7.98717978950973,7.17831007049656));
#17258=CARTESIAN_POINT('Ctrl Pts',(10.0502525316942,8.03941132011983,7.08640986444703));
#17259=CARTESIAN_POINT('Ctrl Pts',(10.0502525316942,8.09869101763159,6.97256625288353));
#17260=CARTESIAN_POINT('Ctrl Pts',(10.0502525316942,8.15552703155277,6.84473975688512));
#17261=CARTESIAN_POINT('Ctrl Pts',(10.0502525316942,8.19531386354866,6.73121306554078));
#17262=CARTESIAN_POINT('Ctrl Pts',(10.0502525316942,8.21862212728407,6.63151085898163));
#17263=CARTESIAN_POINT('Ctrl Pts',(10.0502525316942,8.22655212821854,6.54471580350543));
#17264=CARTESIAN_POINT('Ctrl Pts',(10.0502525316942,8.22086585997457,6.46935831372324));
#17265=CARTESIAN_POINT('Ctrl Pts',(10.0502525316942,8.20424193086582,6.40320361025513));
#17266=CARTESIAN_POINT('Ctrl Pts',(10.0502525316942,8.17999182956336,6.34348879371404));
#17267=CARTESIAN_POINT('Ctrl Pts',(10.0502525316942,8.15151829405778,6.2873754147921));
#17268=CARTESIAN_POINT('Ctrl Pts',(10.0502525316942,8.12184190992835,6.23234494937036));
#17269=CARTESIAN_POINT('Ctrl Pts',(10.0502525316942,8.09313431783932,6.1765889417745));
#17270=CARTESIAN_POINT('Ctrl Pts',(10.0502525316942,8.06615036325875,6.11948306053102));
#17271=CARTESIAN_POINT('Ctrl Pts',(10.0502525316942,8.04053373452353,6.06133545932041));
#17272=CARTESIAN_POINT('Ctrl Pts',(10.0502525316942,8.01529125034138,6.00299507467205));
#17273=CARTESIAN_POINT('Ctrl Pts',(10.0502525316942,7.98919862941808,5.94551682580168));
#17274=CARTESIAN_POINT('Ctrl Pts',(10.0502525316942,7.96124121028423,5.88979801918435));
#17275=CARTESIAN_POINT('Ctrl Pts',(10.0502525316942,7.93101524786534,5.83624706470931));
#17276=CARTESIAN_POINT('Ctrl Pts',(10.0502525316942,7.89853935606421,5.78493261248025));
#17277=CARTESIAN_POINT('Ctrl Pts',(10.0502525316942,7.86408741650604,5.73571509186187));
#17278=CARTESIAN_POINT('Ctrl Pts',(10.0502525316942,7.82802562040593,5.68837508612421));
#17279=CARTESIAN_POINT('Ctrl Pts',(10.0502525316942,7.79062713132508,5.64275916621446));
#17280=CARTESIAN_POINT('Ctrl Pts',(10.0502525316942,7.75196943392054,5.59886036305501));
#17281=CARTESIAN_POINT('Ctrl Pts',(10.0502525316942,7.71201392777609,5.55675475816771));
#17282=CARTESIAN_POINT('Ctrl Pts',(10.0502525316942,7.67064916836037,5.51656644870715));
#17283=CARTESIAN_POINT('Ctrl Pts',(10.0502525316942,7.62774439672625,5.47842458761391));
#17284=CARTESIAN_POINT('Ctrl Pts',(10.0502525316942,7.58320832269043,5.44241518816367));
#17285=CARTESIAN_POINT('Ctrl Pts',(10.0502525316942,7.5369975221287,5.4085767049601));
#17286=CARTESIAN_POINT('Ctrl Pts',(10.0502525316942,7.49867649345608,5.38325149258725));
#17287=CARTESIAN_POINT('Ctrl Pts',(10.0502525316942,7.46917564122634,5.36523734954955));
#17288=CARTESIAN_POINT('Ctrl Pts',(10.0502525316942,7.44917117889019,5.35366260632437));
#17289=CARTESIAN_POINT('Ctrl Pts',(10.0502525316942,7.43908464225652,5.34798390487229));
#17290=CARTESIAN_POINT('',(10.0502525316942,8.06781615908999,4.34180314898733));
#17291=CARTESIAN_POINT('Origin',(10.0502525316942,0.,0.));
#17292=CARTESIAN_POINT('',(10.0502525316942,9.78902788303806,4.46902397810655));
#17293=CARTESIAN_POINT('Ctrl Pts',(10.0502525316942,8.06781615908999,4.34180314898733));
#17294=CARTESIAN_POINT('Ctrl Pts',(10.0502525316942,8.07691891810119,4.34789619493555));
#17295=CARTESIAN_POINT('Ctrl Pts',(10.0502525316942,8.09522509309135,4.35989510698125));
#17296=CARTESIAN_POINT('Ctrl Pts',(10.0502525316942,8.1229863261673,4.37733193665808));
#17297=CARTESIAN_POINT('Ctrl Pts',(10.0502525316942,8.16060634100777,4.39945592264773));
#17298=CARTESIAN_POINT('Ctrl Pts',(10.0502525316942,8.20864682657585,4.42521825196285));
#17299=CARTESIAN_POINT('Ctrl Pts',(10.0502525316942,8.25771295042534,4.44905598790391));
#17300=CARTESIAN_POINT('Ctrl Pts',(10.0502525316942,8.30781651946229,4.47092121748728));
#17301=CARTESIAN_POINT('Ctrl Pts',(10.0502525316942,8.35896957008516,4.49074778380617));
#17302=CARTESIAN_POINT('Ctrl Pts',(10.0502525316942,8.41118223898599,4.50845195831808));
#17303=CARTESIAN_POINT('Ctrl Pts',(10.0502525316942,8.46445618393006,4.52395547727261));
#17304=CARTESIAN_POINT('Ctrl Pts',(10.0502525316942,8.51877787179233,4.53720779434568));
#17305=CARTESIAN_POINT('Ctrl Pts',(10.0502525316942,8.5741121935049,4.54820764638295));
#17306=CARTESIAN_POINT('Ctrl Pts',(10.0502525316942,8.63039414709753,4.557029509662));
#17307=CARTESIAN_POINT('Ctrl Pts',(10.0502525316942,8.68752517632497,4.5638375509418));
#17308=CARTESIAN_POINT('Ctrl Pts',(10.0502525316942,8.7453900186693,4.56884434816008));
#17309=CARTESIAN_POINT('Ctrl Pts',(10.0502525316942,8.80387069695484,4.57227742599473));
#17310=CARTESIAN_POINT('Ctrl Pts',(10.0502525316942,8.86286066111437,4.57434503953799));
#17311=CARTESIAN_POINT('Ctrl Pts',(10.0502525316942,8.92228054501355,4.57519852862449));
#17312=CARTESIAN_POINT('Ctrl Pts',(10.0502525316942,8.98208782772813,4.57490858968921));
#17313=CARTESIAN_POINT('Ctrl Pts',(10.0502525316942,9.0422641588092,4.57349279247872));
#17314=CARTESIAN_POINT('Ctrl Pts',(10.0502525316942,9.10280619261976,4.57093505021141));
#17315=CARTESIAN_POINT('Ctrl Pts',(10.0502525316942,9.16371548601266,4.56720740240461));
#17316=CARTESIAN_POINT('Ctrl Pts',(10.0502525316942,9.22498785759991,4.56229279796226));
#17317=CARTESIAN_POINT('Ctrl Pts',(10.0502525316942,9.28660567396873,4.55620201600645));
#17318=CARTESIAN_POINT('Ctrl Pts',(10.0502525316942,9.34854353993788,4.54896317065147));
#17319=CARTESIAN_POINT('Ctrl Pts',(10.0502525316942,9.4107719162247,4.54061558349964));
#17320=CARTESIAN_POINT('Ctrl Pts',(10.0502525316942,9.47326135298215,4.53120240639841));
#17321=CARTESIAN_POINT('Ctrl Pts',(10.0502525316942,9.53598658803447,4.52076380103831));
#17322=CARTESIAN_POINT('Ctrl Pts',(10.0502525316942,9.59893007547295,4.50933089675096));
#17323=CARTESIAN_POINT('Ctrl Pts',(10.0502525316942,9.6620803346471,4.49692680496291));
#17324=CARTESIAN_POINT('Ctrl Pts',(10.0502525316942,9.71276073586856,4.48623896772408));
#17325=CARTESIAN_POINT('Ctrl Pts',(10.0502525316942,9.7508598377266,4.47779691026849));
#17326=CARTESIAN_POINT('Ctrl Pts',(10.0502525316942,9.77629863524131,4.47197980068818));
#17327=CARTESIAN_POINT('Ctrl Pts',(10.0502525316942,9.78902788303806,4.46902397810655));
#17328=CARTESIAN_POINT('',(10.0502525316942,8.7276078365385,2.78743136471945));
#17329=CARTESIAN_POINT('Ctrl Pts',(10.0502525316942,9.78902788303806,4.46902397810655));
#17330=CARTESIAN_POINT('Ctrl Pts',(10.0502525316942,9.7979092591739,4.43164817642871));
#17331=CARTESIAN_POINT('Ctrl Pts',(10.0502525316942,9.81447918831044,4.35880427644625));
#17332=CARTESIAN_POINT('Ctrl Pts',(10.0502525316942,9.83575560039739,4.25526155603325));
#17333=CARTESIAN_POINT('Ctrl Pts',(10.0502525316942,9.85695433232581,4.12867141346467));
#17334=CARTESIAN_POINT('Ctrl Pts',(10.0502525316942,9.87150803413088,3.98953789729602));
#17335=CARTESIAN_POINT('Ctrl Pts',(10.0502525316942,9.87426588302275,3.86927279048049));
#17336=CARTESIAN_POINT('Ctrl Pts',(10.0502525316942,9.86562368292838,3.76724770763979));
#17337=CARTESIAN_POINT('Ctrl Pts',(10.0502525316942,9.84634441482148,3.68225019949279));
#17338=CARTESIAN_POINT('Ctrl Pts',(10.0502525316942,9.81764970735851,3.61233812130575));
#17339=CARTESIAN_POINT('Ctrl Pts',(10.0502525316942,9.78139648362373,3.55455833609672));
#17340=CARTESIAN_POINT('Ctrl Pts',(10.0502525316942,9.73988037363202,3.50525986412372));
#17341=CARTESIAN_POINT('Ctrl Pts',(10.0502525316942,9.6954604444488,3.46069167580983));
#17342=CARTESIAN_POINT('Ctrl Pts',(10.0502525316942,9.65023117691875,3.41752510010333));
#17343=CARTESIAN_POINT('Ctrl Pts',(10.0502525316942,9.60569908050971,3.37336911957978));
#17344=CARTESIAN_POINT('Ctrl Pts',(10.0502525316942,9.56238912688746,3.32739669964523));
#17345=CARTESIAN_POINT('Ctrl Pts',(10.0502525316942,9.5200576682471,3.28001101822472));
#17346=CARTESIAN_POINT('Ctrl Pts',(10.0502525316942,9.47802246886347,3.23232637183425));
#17347=CARTESIAN_POINT('Ctrl Pts',(10.0502525316942,9.43544515599928,3.18572437199394));
#17348=CARTESIAN_POINT('Ctrl Pts',(10.0502525316942,9.3916380122022,3.14137195551156));
#17349=CARTESIAN_POINT('Ctrl Pts',(10.0502525316942,9.34634325868463,3.09978230736302));
#17350=CARTESIAN_POINT('Ctrl Pts',(10.0502525316942,9.29959981236885,3.0610149656645));
#17351=CARTESIAN_POINT('Ctrl Pts',(10.0502525316942,9.25162502046097,3.02485255677715));
#17352=CARTESIAN_POINT('Ctrl Pts',(10.0502525316942,9.20269934800391,2.99097324368152));
#17353=CARTESIAN_POINT('Ctrl Pts',(10.0502525316942,9.15303517679781,2.95914669449447));
#17354=CARTESIAN_POINT('Ctrl Pts',(10.0502525316942,9.10270404556727,2.92934233715353));
#17355=CARTESIAN_POINT('Ctrl Pts',(10.0502525316942,9.05169275361811,2.9016444576704));
#17356=CARTESIAN_POINT('Ctrl Pts',(10.0502525316942,8.99993365903229,2.87620551770673));
#17357=CARTESIAN_POINT('Ctrl Pts',(10.0502525316942,8.94734231311461,2.85318875574511));
#17358=CARTESIAN_POINT('Ctrl Pts',(10.0502525316942,8.89385847330528,2.83270418548989));
#17359=CARTESIAN_POINT('Ctrl Pts',(10.0502525316942,8.83945272393405,2.81480179823484));
#17360=CARTESIAN_POINT('Ctrl Pts',(10.0502525316942,8.79518133889446,2.80255793908285));
#17361=CARTESIAN_POINT('Ctrl Pts',(10.0502525316942,8.76155768480736,2.7945417356489));
#17362=CARTESIAN_POINT('Ctrl Pts',(10.0502525316942,8.73895551818547,2.78971521950536));
#17363=CARTESIAN_POINT('Ctrl Pts',(10.0502525316942,8.7276078365385,2.78743136471945));
#17364=CARTESIAN_POINT('',(10.0502525316942,9.01464008964162,1.6362078766636));
#17365=CARTESIAN_POINT('Origin',(10.0502525316942,0.,0.));
#17366=CARTESIAN_POINT('',(10.0502525316942,10.6909231138624,1.22531840158854));
#17367=CARTESIAN_POINT('Ctrl Pts',(10.0502525316942,9.01464008964162,1.6362078766636));
#17368=CARTESIAN_POINT('Ctrl Pts',(10.0502525316942,9.02518018266099,1.63918980048658));
#17369=CARTESIAN_POINT('Ctrl Pts',(10.0502525316942,9.04629825740996,1.64494452480213));
#17370=CARTESIAN_POINT('Ctrl Pts',(10.0502525316942,9.07808903572539,1.65294924248453));
#17371=CARTESIAN_POINT('Ctrl Pts',(10.0502525316942,9.12070448363665,1.66236517961207));
#17372=CARTESIAN_POINT('Ctrl Pts',(10.0502525316942,9.17435469805521,1.67202128432359));
#17373=CARTESIAN_POINT('Ctrl Pts',(10.0502525316942,9.22838562038483,1.67953005230647));
#17374=CARTESIAN_POINT('Ctrl Pts',(10.0502525316942,9.28279367373423,1.68484226707077));
#17375=CARTESIAN_POINT('Ctrl Pts',(10.0502525316942,9.33756986179013,1.68789129020751));
#17376=CARTESIAN_POINT('Ctrl Pts',(10.0502525316942,9.39269795157698,1.68859435873067));
#17377=CARTESIAN_POINT('Ctrl Pts',(10.0502525316942,9.44815533489435,1.68687652711276));
#17378=CARTESIAN_POINT('Ctrl Pts',(10.0502525316942,9.50391352130234,1.68269390490855));
#17379=CARTESIAN_POINT('Ctrl Pts',(10.0502525316942,9.55993872975698,1.67605614008548));
#17380=CARTESIAN_POINT('Ctrl Pts',(10.0502525316942,9.61619215414635,1.66705415050613));
#17381=CARTESIAN_POINT('Ctrl Pts',(10.0502525316942,9.67263079222962,1.65587452359108));
#17382=CARTESIAN_POINT('Ctrl Pts',(10.0502525316942,9.72921071303343,1.64275505105007));
#17383=CARTESIAN_POINT('Ctrl Pts',(10.0502525316942,9.78589002258816,1.62794857866286));
#17384=CARTESIAN_POINT('Ctrl Pts',(10.0502525316942,9.84263174012077,1.6116860945735));
#17385=CARTESIAN_POINT('Ctrl Pts',(10.0502525316942,9.89940715053283,1.59413605700217));
#17386=CARTESIAN_POINT('Ctrl Pts',(10.0502525316942,9.9561976604221,1.57537884194225));
#17387=CARTESIAN_POINT('Ctrl Pts',(10.0502525316942,10.0129912468249,1.55543682981628));
#17388=CARTESIAN_POINT('Ctrl Pts',(10.0502525316942,10.0697797567623,1.53429575504446));
#17389=CARTESIAN_POINT('Ctrl Pts',(10.0502525316942,10.1265560306252,1.51192854453357));
#17390=CARTESIAN_POINT('Ctrl Pts',(10.0502525316942,10.1833108225988,1.48832027384755));
#17391=CARTESIAN_POINT('Ctrl Pts',(10.0502525316942,10.2400306932429,1.4634866435649));
#17392=CARTESIAN_POINT('Ctrl Pts',(10.0502525316942,10.2967001780439,1.43746223933981));
#17393=CARTESIAN_POINT('Ctrl Pts',(10.0502525316942,10.353303334518,1.41029358637874));
#17394=CARTESIAN_POINT('Ctrl Pts',(10.0502525316942,10.4098254888505,1.38203082503059));
#17395=CARTESIAN_POINT('Ctrl Pts',(10.0502525316942,10.4662550259293,1.35271995777451));
#17396=CARTESIAN_POINT('Ctrl Pts',(10.0502525316942,10.5225848780961,1.32239601234813));
#17397=CARTESIAN_POINT('Ctrl Pts',(10.0502525316942,10.5788112684272,1.29108451674038));
#17398=CARTESIAN_POINT('Ctrl Pts',(10.0502525316942,10.6237084709174,1.26525867423012));
#17399=CARTESIAN_POINT('Ctrl Pts',(10.0502525316942,10.6573341307832,1.24545653053149));
#17400=CARTESIAN_POINT('Ctrl Pts',(10.0502525316942,10.6797302792078,1.23206310981063));
#17401=CARTESIAN_POINT('Ctrl Pts',(10.0502525316942,10.6909231138624,1.22531840158854));
#17402=CARTESIAN_POINT('',(10.0502525316942,9.16181196696065,-0.0459743785884358));
#17403=CARTESIAN_POINT('Ctrl Pts',(10.0502525316942,10.6909231138624,1.22531840158854));
#17404=CARTESIAN_POINT('Ctrl Pts',(10.0502525316942,10.6878200466132,1.18702740569167));
#17405=CARTESIAN_POINT('Ctrl Pts',(10.0502525316942,10.6810689826619,1.11262835024222));
#17406=CARTESIAN_POINT('Ctrl Pts',(10.0502525316942,10.6693075927691,1.00757859836431));
#17407=CARTESIAN_POINT('Ctrl Pts',(10.0502525316942,10.6503502795328,0.880633449950656));
#17408=CARTESIAN_POINT('Ctrl Pts',(10.0502525316942,10.6211970514875,0.743812271574576));
#17409=CARTESIAN_POINT('Ctrl Pts',(10.0502525316942,10.5866559598108,0.628581135879225));
#17410=CARTESIAN_POINT('Ctrl Pts',(10.0502525316942,10.5469092546456,0.534220102715978));
#17411=CARTESIAN_POINT('Ctrl Pts',(10.0502525316942,10.5023079065862,0.459340290208067));
#17412=CARTESIAN_POINT('Ctrl Pts',(10.0502525316942,10.4534135977985,0.40171710493522));
#17413=CARTESIAN_POINT('Ctrl Pts',(10.0502525316942,10.4010797975679,0.357968125936964));
#17414=CARTESIAN_POINT('Ctrl Pts',(10.0502525316942,10.3463615649927,0.323911676451426));
#17415=CARTESIAN_POINT('Ctrl Pts',(10.0502525316942,10.2903433742921,0.295251323542576));
#17416=CARTESIAN_POINT('Ctrl Pts',(10.0502525316942,10.2339885791981,0.268174082740676));
#17417=CARTESIAN_POINT('Ctrl Pts',(10.0502525316942,10.1779910903389,0.239940424315885));
#17418=CARTESIAN_POINT('Ctrl Pts',(10.0502525316942,10.1225946176937,0.209601566462141));
#17419=CARTESIAN_POINT('Ctrl Pts',(10.0502525316942,10.0676920272606,0.177616245484636));
#17420=CARTESIAN_POINT('Ctrl Pts',(10.0502525316942,10.0129788108676,0.145255042779231));
#17421=CARTESIAN_POINT('Ctrl Pts',(10.0502525316942,9.95808457009925,0.11409102040857));
#17422=CARTESIAN_POINT('Ctrl Pts',(10.0502525316942,9.90271585009609,0.0854465176078907));
#17423=CARTESIAN_POINT('Ctrl Pts',(10.0502525316942,9.84678607154126,0.0598892603187502));
#17424=CARTESIAN_POINT('Ctrl Pts',(10.0502525316942,9.79035064491696,0.0374638466641572));
#17425=CARTESIAN_POINT('Ctrl Pts',(10.0502525316942,9.73354910755133,0.017896378048051));
#17426=CARTESIAN_POINT('Ctrl Pts',(10.0502525316942,9.67654874444263,0.000794100811299831));
#17427=CARTESIAN_POINT('Ctrl Pts',(10.0502525316942,9.61948036621956,-0.0141276732699903));
#17428=CARTESIAN_POINT('Ctrl Pts',(10.0502525316942,9.56240256296547,-0.0269201266367288));
#17429=CARTESIAN_POINT('Ctrl Pts',(10.0502525316942,9.50532882588415,-0.0374990192894116));
#17430=CARTESIAN_POINT('Ctrl Pts',(10.0502525316942,9.44824193693312,-0.0456984490690175));
#17431=CARTESIAN_POINT('Ctrl Pts',(10.0502525316942,9.39111202409575,-0.0513370708710177));
#17432=CARTESIAN_POINT('Ctrl Pts',(10.0502525316942,9.33391578939727,-0.0542916394702416));
#17433=CARTESIAN_POINT('Ctrl Pts',(10.0502525316942,9.27664070503215,-0.0545055203789815));
#17434=CARTESIAN_POINT('Ctrl Pts',(10.0502525316942,9.23075255525014,-0.0524695120683285));
#17435=CARTESIAN_POINT('Ctrl Pts',(10.0502525316942,9.19629741683749,-0.0497030940542379));
#17436=CARTESIAN_POINT('Ctrl Pts',(10.0502525316942,9.17331000347738,-0.0473089300876987));
#17437=CARTESIAN_POINT('Ctrl Pts',(10.0502525316942,9.16181196696065,-0.0459743785884358));
#17438=CARTESIAN_POINT('',(10.0502525316942,9.07904823952839,-1.22955082275859));
#17439=CARTESIAN_POINT('Origin',(10.0502525316942,0.,0.));
#17440=CARTESIAN_POINT('',(10.0502525316942,10.5463163022605,-2.13832987737225));
#17441=CARTESIAN_POINT('Ctrl Pts',(10.0502525316942,9.07904823952839,-1.22955082275859));
#17442=CARTESIAN_POINT('Ctrl Pts',(10.0502525316942,9.08999392881405,-1.22997191254093));
#17443=CARTESIAN_POINT('Ctrl Pts',(10.0502525316942,9.11185671902711,-1.23102468846705));
#17444=CARTESIAN_POINT('Ctrl Pts',(10.0502525316942,9.14456513970113,-1.23323564031797));
#17445=CARTESIAN_POINT('Ctrl Pts',(10.0502525316942,9.18800452372235,-1.23744944958329));
#17446=CARTESIAN_POINT('Ctrl Pts',(10.0502525316942,9.24201281020108,-1.24484477628256));
#17447=CARTESIAN_POINT('Ctrl Pts',(10.0502525316942,9.29571960787763,-1.2543999867847));
#17448=CARTESIAN_POINT('Ctrl Pts',(10.0502525316942,9.34910630619445,-1.26616078343298));
#17449=CARTESIAN_POINT('Ctrl Pts',(10.0502525316942,9.40214375674832,-1.28018776310679));
#17450=CARTESIAN_POINT('Ctrl Pts',(10.0502525316942,9.45479094589287,-1.29655462181801));
#17451=CARTESIAN_POINT('Ctrl Pts',(10.0502525316942,9.50700321251013,-1.31532565068075));
#17452=CARTESIAN_POINT('Ctrl Pts',(10.0502525316942,9.55873989768809,-1.33653378795886));
#17453=CARTESIAN_POINT('Ctrl Pts',(10.0502525316942,9.60997185513068,-1.36015941897336));
#17454=CARTESIAN_POINT('Ctrl Pts',(10.0502525316942,9.6606902731969,-1.38610408395052));
#17455=CARTESIAN_POINT('Ctrl Pts',(10.0502525316942,9.7109119130093,-1.41417703928493));
#17456=CARTESIAN_POINT('Ctrl Pts',(10.0502525316942,9.76066847540881,-1.44413855620418));
#17457=CARTESIAN_POINT('Ctrl Pts',(10.0502525316942,9.80999825050556,-1.47573521813323));
#17458=CARTESIAN_POINT('Ctrl Pts',(10.0502525316942,9.85893744675637,-1.50873591460517));
#17459=CARTESIAN_POINT('Ctrl Pts',(10.0502525316942,9.90751081093262,-1.54297155887855));
#17460=CARTESIAN_POINT('Ctrl Pts',(10.0502525316942,9.95572549720588,-1.57835996316384));
#17461=CARTESIAN_POINT('Ctrl Pts',(10.0502525316942,10.003576986989,-1.61487612711423));
#17462=CARTESIAN_POINT('Ctrl Pts',(10.0502525316942,10.0510531180319,-1.65253109869336));
#17463=CARTESIAN_POINT('Ctrl Pts',(10.0502525316942,10.0981387150956,-1.69134841350201));
#17464=CARTESIAN_POINT('Ctrl Pts',(10.0502525316942,10.1448203729832,-1.73133940840847));
#17465=CARTESIAN_POINT('Ctrl Pts',(10.0502525316942,10.1910901617733,-1.77248499825981));
#17466=CARTESIAN_POINT('Ctrl Pts',(10.0502525316942,10.2369440613944,-1.81474751134677));
#17467=CARTESIAN_POINT('Ctrl Pts',(10.0502525316942,10.2823812867227,-1.85807777307013));
#17468=CARTESIAN_POINT('Ctrl Pts',(10.0502525316942,10.3274033763511,-1.90242356266618));
#17469=CARTESIAN_POINT('Ctrl Pts',(10.0502525316942,10.3720134991994,-1.94773753991041));
#17470=CARTESIAN_POINT('Ctrl Pts',(10.0502525316942,10.4162157576914,-1.99398420741813));
#17471=CARTESIAN_POINT('Ctrl Pts',(10.0502525316942,10.4600144483414,-2.04113811949547));
#17472=CARTESIAN_POINT('Ctrl Pts',(10.0502525316942,10.4947336011034,-2.07957395387303));
#17473=CARTESIAN_POINT('Ctrl Pts',(10.0502525316942,10.5205943051056,-2.10879781201984));
#17474=CARTESIAN_POINT('Ctrl Pts',(10.0502525316942,10.5377555133892,-2.12845650254365));
#17475=CARTESIAN_POINT('Ctrl Pts',(10.0502525316942,10.5463163022605,-2.13832987737225));
#17476=CARTESIAN_POINT('Ctrl Pts',(10.0502525316942,10.5463163022605,-2.13832987737225));
#17477=CARTESIAN_POINT('Ctrl Pts',(10.0502525316942,10.531532541469,-2.17378787802072));
#17478=CARTESIAN_POINT('Ctrl Pts',(10.0502525316942,10.5021213256069,-2.24245939102107));
#17479=CARTESIAN_POINT('Ctrl Pts',(10.0502525316942,10.4584734205235,-2.33873317272541));
#17480=CARTESIAN_POINT('Ctrl Pts',(10.0502525316942,10.4012157360254,-2.45360705137856));
#17481=CARTESIAN_POINT('Ctrl Pts',(10.0502525316942,10.3312092992132,-2.57472288173342));
#17482=CARTESIAN_POINT('Ctrl Pts',(10.0502525316942,10.2627503896831,-2.6736404198842));
#17483=CARTESIAN_POINT('Ctrl Pts',(10.0502525316942,10.1957898638803,-2.751100687992));
#17484=CARTESIAN_POINT('Ctrl Pts',(10.0502525316942,10.1302323265723,-2.80853304709422));
#17485=CARTESIAN_POINT('Ctrl Pts',(10.0502525316942,10.0659245320707,-2.84822678059402));
#17486=CARTESIAN_POINT('Ctrl Pts',(10.0502525316942,10.0026329523419,-2.8736624985001));
#17487=CARTESIAN_POINT('Ctrl Pts',(10.0502525316942,9.94006879903196,-2.88914324293729));
#17488=CARTESIAN_POINT('Ctrl Pts',(10.0502525316942,9.8779357976215,-2.89909028540996));
#17489=CARTESIAN_POINT('Ctrl Pts',(10.0502525316942,9.81597187495431,-2.90742768231934));
#17490=CARTESIAN_POINT('Ctrl Pts',(10.0502525316942,9.753990418012,-2.91697531144329));
#17491=CARTESIAN_POINT('Ctrl Pts',(10.0502525316942,9.69193001905628,-2.92871082842625));
#17492=CARTESIAN_POINT('Ctrl Pts',(10.0502525316942,9.62983054491074,-2.94216484288864));
#17493=CARTESIAN_POINT('Ctrl Pts',(10.0502525316942,9.56779502233835,-2.95603486191442));
#17494=CARTESIAN_POINT('Ctrl Pts',(10.0502525316942,9.50595728442294,-2.96871035517328));
#17495=CARTESIAN_POINT('Ctrl Pts',(10.0502525316942,9.44444686430419,-2.97884302078014));
#17496=CARTESIAN_POINT('Ctrl Pts',(10.0502525316942,9.38335685712271,-2.98586616479853));
#17497=CARTESIAN_POINT('Ctrl Pts',(10.0502525316942,9.32275374295661,-2.98975449467364));
#17498=CARTESIAN_POINT('Ctrl Pts',(10.0502525316942,9.26268559037018,-2.99081162285579));
#17499=CARTESIAN_POINT('Ctrl Pts',(10.0502525316942,9.20319012929579,-2.98946277417915));
#17500=CARTESIAN_POINT('Ctrl Pts',(10.0502525316942,9.144303794535,-2.9860191259415));
#17501=CARTESIAN_POINT('Ctrl Pts',(10.0502525316942,9.08606649232432,-2.98054746086824));
#17502=CARTESIAN_POINT('Ctrl Pts',(10.0502525316942,9.02851708515246,-2.97297183097014));
#17503=CARTESIAN_POINT('Ctrl Pts',(10.0502525316942,8.97169046427448,-2.96312913325008));
#17504=CARTESIAN_POINT('Ctrl Pts',(10.0502525316942,8.91561425843345,-2.95083766730389));
#17505=CARTESIAN_POINT('Ctrl Pts',(10.0502525316942,8.86030439480771,-2.93597302048693));
#17506=CARTESIAN_POINT('Ctrl Pts',(10.0502525316942,8.80576645976534,-2.91847745889582));
#17507=CARTESIAN_POINT('Ctrl Pts',(10.0502525316942,8.76275339706311,-2.90236088180168));
#17508=CARTESIAN_POINT('Ctrl Pts',(10.0502525316942,8.7308394833358,-2.88908263860953));
#17509=CARTESIAN_POINT('Ctrl Pts',(10.0502525316942,8.70971699141988,-2.87970215198308));
#17510=CARTESIAN_POINT('Ctrl Pts',(10.0502525316942,8.69919410795919,-2.87487982939776));
#17511=CARTESIAN_POINT('Origin',(29.1,0.,0.));
#17512=CARTESIAN_POINT('',(29.35,6.525,7.99082036443648E-16));
#17513=CARTESIAN_POINT('',(29.1,6.275,-7.68465866464964E-16));
#17514=CARTESIAN_POINT('Origin',(29.35,0.,0.));
#17515=CARTESIAN_POINT('Origin',(29.35,6.025,0.));
#17516=CARTESIAN_POINT('',(29.35,9.5,-1.16341445918999E-15));
#17517=CARTESIAN_POINT('Origin',(29.35,0.,0.));
#17518=CARTESIAN_POINT('Origin',(29.1,0.,0.));
#17519=CARTESIAN_POINT('',(28.85,10.,1.22464679914735E-15));
#17520=CARTESIAN_POINT('',(29.1,9.75,1.19403062916867E-15));
#17521=CARTESIAN_POINT('',(28.85,-10.,-1.22464679914735E-15));
#17522=CARTESIAN_POINT('Origin',(28.85,0.,0.));
#17523=CARTESIAN_POINT('Origin',(28.85,0.,0.));
#17524=CARTESIAN_POINT('Origin',(25.175,0.,0.));
#17525=CARTESIAN_POINT('',(25.175,-10.,-1.22464679914735E-15));
#17526=CARTESIAN_POINT('',(21.,-10.,-1.22464679914735E-15));
#17527=CARTESIAN_POINT('',(25.175,-10.,-1.22464679914735E-15));
#17528=CARTESIAN_POINT('Origin',(21.,0.,0.));
#17529=CARTESIAN_POINT('Origin',(15.75,0.,0.));
#17530=CARTESIAN_POINT('',(14.657256909085,15.6550387777217,-0.574937672128248));
#17531=CARTESIAN_POINT('',(15.8,14.2136654476498,-2.58416182157067));
#17532=CARTESIAN_POINT('Ctrl Pts',(14.657256909085,15.6550387777217,-0.574937672128247));
#17533=CARTESIAN_POINT('Ctrl Pts',(14.6763724381383,15.6262431452138,-0.80344402932419));
#17534=CARTESIAN_POINT('Ctrl Pts',(14.6998065311113,15.5861385521166,-1.05535166589827));
#17535=CARTESIAN_POINT('Ctrl Pts',(14.7651359522577,15.4797512169027,-1.49901297546982));
#17536=CARTESIAN_POINT('Ctrl Pts',(14.7991842945127,15.4284906283794,-1.63134031220526));
#17537=CARTESIAN_POINT('Ctrl Pts',(14.8880411294635,15.3057468955346,-1.8758277497676));
#17538=CARTESIAN_POINT('Ctrl Pts',(14.9527298447847,15.2276701479799,-1.94065298884131));
#17539=CARTESIAN_POINT('Ctrl Pts',(15.1817050684316,14.9444552503125,-2.21319070454604));
#17540=CARTESIAN_POINT('Ctrl Pts',(15.241493513239,14.8626126835113,-2.32251843283214));
#17541=CARTESIAN_POINT('Ctrl Pts',(15.4262634482943,14.6383589683629,-2.47073976049445));
#17542=CARTESIAN_POINT('Ctrl Pts',(15.4835457818315,14.5700757971062,-2.5074724098941));
#17543=CARTESIAN_POINT('Ctrl Pts',(15.6181084961337,14.4133333652787,-2.57062182851529));
#17544=CARTESIAN_POINT('Ctrl Pts',(15.7034661294672,14.3167713861451,-2.59269541157918));
#17545=CARTESIAN_POINT('Ctrl Pts',(15.8,14.2136654476498,-2.58416182157067));
#17546=CARTESIAN_POINT('',(15.8,14.4464654837189,0.0762417569101993));
#17547=CARTESIAN_POINT('Ctrl Pts',(15.8,14.4464654837189,0.0762417569101992));
#17548=CARTESIAN_POINT('Ctrl Pts',(15.7480221813552,14.5017894200628,0.0989497576662197));
#17549=CARTESIAN_POINT('Ctrl Pts',(15.6946673265391,14.55856814069,0.115136586527327));
#17550=CARTESIAN_POINT('Ctrl Pts',(15.5889287876155,14.6712292799262,0.130653500227229));
#17551=CARTESIAN_POINT('Ctrl Pts',(15.5369709165892,14.7266555496971,0.130547397724583));
#17552=CARTESIAN_POINT('Ctrl Pts',(15.4102920065978,14.8619679647836,0.108175767558855));
#17553=CARTESIAN_POINT('Ctrl Pts',(15.3183831004347,14.9605133746384,0.0733004344337784));
#17554=CARTESIAN_POINT('Ctrl Pts',(15.0640351589848,15.2315511945023,-0.110790343309231));
#17555=CARTESIAN_POINT('Ctrl Pts',(14.8841363199333,15.424113326113,-0.268817147256488));
#17556=CARTESIAN_POINT('Ctrl Pts',(14.657256909085,15.6550387777217,-0.574937672128247));
#17557=CARTESIAN_POINT('Origin',(15.8,0.,0.));
#17558=CARTESIAN_POINT('Origin',(15.75,0.,0.));
#17559=CARTESIAN_POINT('',(14.657256909085,15.0664921537995,4.29087481037367));
#17560=CARTESIAN_POINT('',(15.8,14.3165490635069,1.93458023611785));
#17561=CARTESIAN_POINT('Ctrl Pts',(14.657256909085,15.0664921537995,4.29087481037367));
#17562=CARTESIAN_POINT('Ctrl Pts',(14.6763724381383,15.1097182275582,4.06465401053977));
#17563=CARTESIAN_POINT('Ctrl Pts',(14.6998065311111,15.1494202336739,3.81268261045276));
#17564=CARTESIAN_POINT('Ctrl Pts',(14.7651359522566,15.1853387496715,3.35786013639478));
#17565=CARTESIAN_POINT('Ctrl Pts',(14.799184294511,15.1774784288,3.21616896751162));
#17566=CARTESIAN_POINT('Ctrl Pts',(14.8880411294635,15.136292974961,2.94571769745758));
#17567=CARTESIAN_POINT('Ctrl Pts',(14.9527298447853,15.0820696759655,2.85993818955593));
#17568=CARTESIAN_POINT('Ctrl Pts',(15.1817050684299,14.8969350877898,2.51322120266238));
#17569=CARTESIAN_POINT('Ctrl Pts',(15.2414935132389,14.8528823073187,2.38395361025704));
#17570=CARTESIAN_POINT('Ctrl Pts',(15.4262634482944,14.6854072593997,2.17368854169722));
#17571=CARTESIAN_POINT('Ctrl Pts',(15.483545781832,14.6318171173353,2.11765305577633));
#17572=CARTESIAN_POINT('Ctrl Pts',(15.618108496126,14.5022604497125,2.00915831452887));
#17573=CARTESIAN_POINT('Ctrl Pts',(15.7034661294598,14.417245662525,1.95832579695071));
#17574=CARTESIAN_POINT('Ctrl Pts',(15.8,14.3165490635069,1.93458023611785));
#17575=CARTESIAN_POINT('',(15.8,13.7158451371576,4.53671356284346));
#17576=CARTESIAN_POINT('Ctrl Pts',(15.8,13.7158451371576,4.53671356284347));
#17577=CARTESIAN_POINT('Ctrl Pts',(15.748022181354,13.7614441691838,4.57540619146144));
#17578=CARTESIAN_POINT('Ctrl Pts',(15.6946673265388,13.8104419362193,4.60834637011984));
#17579=CARTESIAN_POINT('Ctrl Pts',(15.5889287876157,13.9127940567891,4.6579180386363));
#17580=CARTESIAN_POINT('Ctrl Pts',(15.5369709165892,13.9655403593053,4.67494478845388));
#17581=CARTESIAN_POINT('Ctrl Pts',(15.4102920065987,14.101143327321,4.69548193961612));
#17582=CARTESIAN_POINT('Ctrl Pts',(15.3183831004355,14.2056426521345,4.69276573315276));
#17583=CARTESIAN_POINT('Ctrl Pts',(15.0640351589826,14.5203021157126,4.60144029184562));
#17584=CARTESIAN_POINT('Ctrl Pts',(14.8841363199283,14.7522725537633,4.51065284133898));
#17585=CARTESIAN_POINT('Ctrl Pts',(14.657256909085,15.0664921537995,4.29087481037367));
#17586=CARTESIAN_POINT('Origin',(15.8,0.,0.));
#17587=CARTESIAN_POINT('Origin',(15.75,0.,0.));
#17588=CARTESIAN_POINT('',(14.657256909085,13.00313230344,8.73666657015347));
#17589=CARTESIAN_POINT('',(15.8,13.0180291077652,6.26395210128207));
#17590=CARTESIAN_POINT('Ctrl Pts',(14.657256909085,13.00313230344,8.73666657015347));
#17591=CARTESIAN_POINT('Ctrl Pts',(14.6763724381384,13.1141488141925,8.53487539574017));
#17592=CARTESIAN_POINT('Ctrl Pts',(14.6998065311113,13.2297711105426,8.307504948367));
#17593=CARTESIAN_POINT('Ctrl Pts',(14.7651359522578,13.4044795231469,7.88604250250778));
#17594=CARTESIAN_POINT('Ctrl Pts',(14.7991842945128,13.4407888928981,7.74885722031068));
#17595=CARTESIAN_POINT('Ctrl Pts',(14.8880411294636,13.4851932372434,7.4789157724344));
#17596=CARTESIAN_POINT('Ctrl Pts',(14.9527298447847,13.4601311411101,7.38057869159978));
#17597=CARTESIAN_POINT('Ctrl Pts',(15.1817050684307,13.3911991258219,6.99362150790972));
#17598=CARTESIAN_POINT('Ctrl Pts',(15.2414935132379,13.3892483247697,6.85706766399487));
#17599=CARTESIAN_POINT('Ctrl Pts',(15.4262634482922,13.294945568639,6.60534106445171));
#17600=CARTESIAN_POINT('Ctrl Pts',(15.4835457818296,13.2612942322572,6.5354878857941));
#17601=CARTESIAN_POINT('Ctrl Pts',(15.6181084961386,13.1716052381211,6.39226804310028));
#17602=CARTESIAN_POINT('Ctrl Pts',(15.7034661294722,13.1064594825804,6.3176524320107));
#17603=CARTESIAN_POINT('Ctrl Pts',(15.8,13.0180291077652,6.26395210128207));
#17604=CARTESIAN_POINT('',(15.8,11.642622304659,8.55310023610356));
#17605=CARTESIAN_POINT('Ctrl Pts',(15.8,11.642622304659,8.55310023610356));
#17606=CARTESIAN_POINT('Ctrl Pts',(15.7480221813541,11.6740328814042,8.60398998850625));
#17607=CARTESIAN_POINT('Ctrl Pts',(15.6946673265388,11.7104534520241,8.65045910276782));
#17608=CARTESIAN_POINT('Ctrl Pts',(15.5889287876158,11.7924776152374,8.72923310580032));
#17609=CARTESIAN_POINT('Ctrl Pts',(15.5369709165892,11.8373807749034,8.76172601103367));
#17610=CARTESIAN_POINT('Ctrl Pts',(15.4102920066149,11.9600005325229,8.82316162406934));
#17611=CARTESIAN_POINT('Ctrl Pts',(15.3183831004502,12.0602246502893,8.85287042548813));
#17612=CARTESIAN_POINT('Ctrl Pts',(15.0640351591008,12.3877046967887,8.86324989111168));
#17613=CARTESIAN_POINT('Ctrl Pts',(14.8841363200439,12.6363765585323,8.84858870232169));
#17614=CARTESIAN_POINT('Ctrl Pts',(14.657256909085,13.00313230344,8.73666657015347));
#17615=CARTESIAN_POINT('Origin',(15.8,0.,0.));
#17616=CARTESIAN_POINT('Origin',(15.75,0.,0.));
#17617=CARTESIAN_POINT('',(14.657256909085,9.66693526506972,12.3272525341113));
#17618=CARTESIAN_POINT('',(15.8,10.4452137610132,9.98016469125221));
#17619=CARTESIAN_POINT('Ctrl Pts',(14.657256909085,9.66693526506972,12.3272525341113));
#17620=CARTESIAN_POINT('Ctrl Pts',(14.6763724381382,9.83487514324392,12.1696437112352));
#17621=CARTESIAN_POINT('Ctrl Pts',(14.6998065311108,10.0150998138711,11.9891308201514));
#17622=CARTESIAN_POINT('Ctrl Pts',(14.7651359522559,10.3114964463889,11.6422840832027));
#17623=CARTESIAN_POINT('Ctrl Pts',(14.7991842945103,10.3884212926728,11.5230333389365));
#17624=CARTESIAN_POINT('Ctrl Pts',(14.8880411294629,10.5140688285991,11.2800254629353));
#17625=CARTESIAN_POINT('Ctrl Pts',(14.9527298447851,10.5206211879139,11.1787567277932));
#17626=CARTESIAN_POINT('Ctrl Pts',(15.1817050684339,10.5746392914499,10.7894374125313));
#17627=CARTESIAN_POINT('Ctrl Pts',(15.2414935132424,10.6149814278139,10.6589641587713));
#17628=CARTESIAN_POINT('Ctrl Pts',(15.4262634482973,10.6030819742843,10.3904167816911));
#17629=CARTESIAN_POINT('Ctrl Pts',(15.4835457818349,10.5926634708524,10.3135836261195));
#17630=CARTESIAN_POINT('Ctrl Pts',(15.6181084961163,10.5516215338708,10.1496580381011));
#17631=CARTESIAN_POINT('Ctrl Pts',(15.7034661294501,10.5127217304364,10.0585632293736));
#17632=CARTESIAN_POINT('Ctrl Pts',(15.8,10.4452137610132,9.98016469125221));
#17633=CARTESIAN_POINT('',(15.8,8.42973848206085,11.7322498653004));
#17634=CARTESIAN_POINT('Ctrl Pts',(15.8,8.42973848206085,11.7322498653004));
#17635=CARTESIAN_POINT('Ctrl Pts',(15.7480221813568,8.44388591742224,11.79035529795));
#17636=CARTESIAN_POINT('Ctrl Pts',(15.6946673265394,8.46416419241759,11.8458046271437));
#17637=CARTESIAN_POINT('Ctrl Pts',(15.5889287876157,8.51783130168368,11.9460700164254));
#17638=CARTESIAN_POINT('Ctrl Pts',(15.5369709165892,8.55049588437244,11.9908484451188));
#17639=CARTESIAN_POINT('Ctrl Pts',(15.4102920066131,8.64812955539648,12.0871687741808));
#17640=CARTESIAN_POINT('Ctrl Pts',(15.3183831004487,8.73426783116772,12.1463944789968));
#17641=CARTESIAN_POINT('Ctrl Pts',(15.0640351590996,9.04251243207698,12.2574628371007));
#17642=CARTESIAN_POINT('Ctrl Pts',(14.8841363200498,9.28354398309004,12.3203630492662));
#17643=CARTESIAN_POINT('Ctrl Pts',(14.657256909085,9.66693526506972,12.3272525341113));
#17644=CARTESIAN_POINT('Origin',(15.8,0.,0.));
#17645=CARTESIAN_POINT('Origin',(15.75,0.,0.));
#17646=CARTESIAN_POINT('',(14.657256909085,5.38447124945594,14.7111611310115));
#17647=CARTESIAN_POINT('',(15.8,6.84994811524973,12.7194492253464));
#17648=CARTESIAN_POINT('Ctrl Pts',(14.657256909085,5.38447124945594,14.7111611310115));
#17649=CARTESIAN_POINT('Ctrl Pts',(14.6763724381383,5.59289536967339,14.6131625093778));
#17650=CARTESIAN_POINT('Ctrl Pts',(14.6998065311112,5.82008076812136,14.4971770340655));
#17651=CARTESIAN_POINT('Ctrl Pts',(14.7651359522584,6.20915225305531,14.2588977812518));
#17652=CARTESIAN_POINT('Ctrl Pts',(14.799184294514,6.31916263594444,14.1692546686358));
#17653=CARTESIAN_POINT('Ctrl Pts',(14.8880411294634,6.51375410718549,13.9769676685644));
#17654=CARTESIAN_POINT('Ctrl Pts',(14.9527298447846,6.55127953136691,13.8826801684932));
#17655=CARTESIAN_POINT('Ctrl Pts',(15.181705068432,6.72296008538512,13.5291080087931));
#17656=CARTESIAN_POINT('Ctrl Pts',(15.2414935132389,6.80164618977777,13.4174869763306));
#17657=CARTESIAN_POINT('Ctrl Pts',(15.4262634482928,6.87331484027241,13.1584061100604));
#17658=CARTESIAN_POINT('Ctrl Pts',(15.4835457818303,6.88714900549683,13.08211394217));
#17659=CARTESIAN_POINT('Ctrl Pts',(15.6181084961339,6.89877159640274,12.9135287874598));
#17660=CARTESIAN_POINT('Ctrl Pts',(15.7034661294676,6.88992552885059,12.814871775685));
#17661=CARTESIAN_POINT('Ctrl Pts',(15.8,6.84994811524973,12.7194492253464));
#17662=CARTESIAN_POINT('',(15.8,4.39169312339699,13.7629651342901));
#17663=CARTESIAN_POINT('Ctrl Pts',(15.8,4.391693123397,13.7629651342901));
#17664=CARTESIAN_POINT('Ctrl Pts',(15.7480221813548,4.3871925678319,13.8225984825995));
#17665=CARTESIAN_POINT('Ctrl Pts',(15.6946673265391,4.3893435683581,13.8816002600415));
#17666=CARTESIAN_POINT('Ctrl Pts',(15.5889287876156,4.40940031310063,13.9935423606787));
#17667=CARTESIAN_POINT('Ctrl Pts',(15.5369709165893,4.42662888187114,14.0462230882418));
#17668=CARTESIAN_POINT('Ctrl Pts',(15.41029200661,4.48971940232603,14.1679996284208));
#17669=CARTESIAN_POINT('Ctrl Pts',(15.3183831004461,4.55334002150981,14.2509448119967));
#17670=CARTESIAN_POINT('Ctrl Pts',(15.064035159032,4.81217604769203,14.4518299178822));
#17671=CARTESIAN_POINT('Ctrl Pts',(14.8841363199712,5.02197344046365,14.5861344199722));
#17672=CARTESIAN_POINT('Ctrl Pts',(14.657256909085,5.38447124945594,14.7111611310115));
#17673=CARTESIAN_POINT('Origin',(15.8,0.,0.));
#17674=CARTESIAN_POINT('Origin',(15.75,0.,0.));
#17675=CARTESIAN_POINT('',(14.657256909085,0.574937672128249,15.6550387777217));
#17676=CARTESIAN_POINT('',(15.8,2.58416182157067,14.2136654476498));
#17677=CARTESIAN_POINT('Ctrl Pts',(14.657256909085,0.574937672128248,15.6550387777217));
#17678=CARTESIAN_POINT('Ctrl Pts',(14.6763724381383,0.803444029323373,15.6262431452139));
#17679=CARTESIAN_POINT('Ctrl Pts',(14.6998065311111,1.05535166589663,15.5861385521169));
#17680=CARTESIAN_POINT('Ctrl Pts',(14.7651359522555,1.49901297545523,15.4797512169063));
#17681=CARTESIAN_POINT('Ctrl Pts',(14.7991842945089,1.63134031219408,15.4284906283848));
#17682=CARTESIAN_POINT('Ctrl Pts',(14.8880411294632,1.87582774976802,15.3057468955349));
#17683=CARTESIAN_POINT('Ctrl Pts',(14.9527298447857,1.94065298884221,15.2276701479787));
#17684=CARTESIAN_POINT('Ctrl Pts',(15.1817050684304,2.21319070454514,14.9444552503138));
#17685=CARTESIAN_POINT('Ctrl Pts',(15.2414935132402,2.32251843283394,14.8626126835097));
#17686=CARTESIAN_POINT('Ctrl Pts',(15.4262634482963,2.47073976049573,14.6383589683605));
#17687=CARTESIAN_POINT('Ctrl Pts',(15.4835457818332,2.50747240989508,14.5700757971041));
#17688=CARTESIAN_POINT('Ctrl Pts',(15.6181084961336,2.57062182851507,14.4133333652788));
#17689=CARTESIAN_POINT('Ctrl Pts',(15.703466129467,2.59269541157921,14.3167713861453));
#17690=CARTESIAN_POINT('Ctrl Pts',(15.8,2.58416182157067,14.2136654476498));
#17691=CARTESIAN_POINT('',(15.8,-0.0762417569101978,14.4464654837189));
#17692=CARTESIAN_POINT('Ctrl Pts',(15.8,-0.0762417569101987,14.4464654837189));
#17693=CARTESIAN_POINT('Ctrl Pts',(15.7480221813551,-0.0989497576662681,
14.5017894200629));
#17694=CARTESIAN_POINT('Ctrl Pts',(15.6946673265391,-0.115136586527329,
14.55856814069));
#17695=CARTESIAN_POINT('Ctrl Pts',(15.5889287876155,-0.130653500227236,
14.6712292799263));
#17696=CARTESIAN_POINT('Ctrl Pts',(15.5369709165891,-0.130547397724572,
14.7266555496972));
#17697=CARTESIAN_POINT('Ctrl Pts',(15.4102920065971,-0.10817576755874,14.8619679647843));
#17698=CARTESIAN_POINT('Ctrl Pts',(15.3183831004339,-0.0733004344332546,
14.9605133746391));
#17699=CARTESIAN_POINT('Ctrl Pts',(15.0640351589857,0.110790343308599,15.2315511945014));
#17700=CARTESIAN_POINT('Ctrl Pts',(14.8841363199342,0.268817147255368,15.4241133261121));
#17701=CARTESIAN_POINT('Ctrl Pts',(14.657256909085,0.574937672128248,15.6550387777217));
#17702=CARTESIAN_POINT('Origin',(15.8,0.,0.));
#17703=CARTESIAN_POINT('Origin',(15.75,0.,0.));
#17704=CARTESIAN_POINT('',(14.657256909085,-4.29087481037367,15.0664921537995));
#17705=CARTESIAN_POINT('',(15.8,-1.93458023611785,14.3165490635069));
#17706=CARTESIAN_POINT('Ctrl Pts',(14.657256909085,-4.29087481037367,15.0664921537995));
#17707=CARTESIAN_POINT('Ctrl Pts',(14.6763724381383,-4.0646540105399,15.1097182275582));
#17708=CARTESIAN_POINT('Ctrl Pts',(14.6998065311111,-3.81268261045262,15.1494202336739));
#17709=CARTESIAN_POINT('Ctrl Pts',(14.7651359522567,-3.35786013639414,15.1853387496715));
#17710=CARTESIAN_POINT('Ctrl Pts',(14.7991842945111,-3.21616896751135,15.1774784288));
#17711=CARTESIAN_POINT('Ctrl Pts',(14.8880411294633,-2.94571769745804,15.1362929749611));
#17712=CARTESIAN_POINT('Ctrl Pts',(14.952729844785,-2.85993818955639,15.0820696759657));
#17713=CARTESIAN_POINT('Ctrl Pts',(15.1817050684315,-2.51322120266002,14.8969350877885));
#17714=CARTESIAN_POINT('Ctrl Pts',(15.2414935132395,-2.3839536102566,14.8528823073182));
#17715=CARTESIAN_POINT('Ctrl Pts',(15.4262634482938,-2.17368854169781,14.6854072594003));
#17716=CARTESIAN_POINT('Ctrl Pts',(15.4835457818316,-2.11765305577666,14.6318171173356));
#17717=CARTESIAN_POINT('Ctrl Pts',(15.6181084961252,-2.00915831452951,14.5022604497133));
#17718=CARTESIAN_POINT('Ctrl Pts',(15.703466129459,-1.9583257969509,14.4172456625258));
#17719=CARTESIAN_POINT('Ctrl Pts',(15.8,-1.93458023611785,14.3165490635069));
#17720=CARTESIAN_POINT('',(15.8,-4.53671356284346,13.7158451371576));
#17721=CARTESIAN_POINT('Ctrl Pts',(15.8,-4.53671356284346,13.7158451371576));
#17722=CARTESIAN_POINT('Ctrl Pts',(15.7480221813549,-4.57540619146074,13.761444169183));
#17723=CARTESIAN_POINT('Ctrl Pts',(15.6946673265391,-4.60834637011968,13.810441936219));
#17724=CARTESIAN_POINT('Ctrl Pts',(15.5889287876154,-4.65791803863646,13.9127940567894));
#17725=CARTESIAN_POINT('Ctrl Pts',(15.5369709165891,-4.6749447884539,13.9655403593054));
#17726=CARTESIAN_POINT('Ctrl Pts',(15.4102920065921,-4.69548193961718,14.1011433273281));
#17727=CARTESIAN_POINT('Ctrl Pts',(15.3183831004293,-4.69276573315053,14.2056426521421));
#17728=CARTESIAN_POINT('Ctrl Pts',(15.0640351589376,-4.60144029182949,14.5203021157682));
#17729=CARTESIAN_POINT('Ctrl Pts',(14.8841363198831,-4.51065284129522,14.7522725538258));
#17730=CARTESIAN_POINT('Ctrl Pts',(14.657256909085,-4.29087481037367,15.0664921537995));
#17731=CARTESIAN_POINT('Origin',(15.8,0.,0.));
#17732=CARTESIAN_POINT('Origin',(15.75,0.,0.));
#17733=CARTESIAN_POINT('',(14.657256909085,-8.73666657015347,13.00313230344));
#17734=CARTESIAN_POINT('',(15.8,-6.26395210128207,13.0180291077652));
#17735=CARTESIAN_POINT('Ctrl Pts',(14.657256909085,-8.73666657015347,13.00313230344));
#17736=CARTESIAN_POINT('Ctrl Pts',(14.6763724381384,-8.53487539574048,13.1141488141923));
#17737=CARTESIAN_POINT('Ctrl Pts',(14.6998065311113,-8.30750494836773,13.2297711105422));
#17738=CARTESIAN_POINT('Ctrl Pts',(14.7651359522579,-7.88604250250723,13.4044795231472));
#17739=CARTESIAN_POINT('Ctrl Pts',(14.7991842945131,-7.74885722031004,13.4407888928982));
#17740=CARTESIAN_POINT('Ctrl Pts',(14.8880411294634,-7.47891577243505,13.4851932372433));
#17741=CARTESIAN_POINT('Ctrl Pts',(14.952729844784,-7.38057869160082,13.4601311411102));
#17742=CARTESIAN_POINT('Ctrl Pts',(15.1817050684321,-6.99362150790738,13.3911991258215));
#17743=CARTESIAN_POINT('Ctrl Pts',(15.241493513237,-6.85706766399776,13.3892483247691));
#17744=CARTESIAN_POINT('Ctrl Pts',(15.4262634482865,-6.60534106445877,13.2949455686422));
#17745=CARTESIAN_POINT('Ctrl Pts',(15.483545781826,-6.53548788579804,13.2612942322595));
#17746=CARTESIAN_POINT('Ctrl Pts',(15.6181084961187,-6.39226804312133,13.1716052381345));
#17747=CARTESIAN_POINT('Ctrl Pts',(15.7034661294532,-6.31765243202127,13.1064594825978));
#17748=CARTESIAN_POINT('Ctrl Pts',(15.8,-6.26395210128207,13.0180291077652));
#17749=CARTESIAN_POINT('',(15.8,-8.55310023610356,11.642622304659));
#17750=CARTESIAN_POINT('Ctrl Pts',(15.8,-8.55310023610356,11.642622304659));
#17751=CARTESIAN_POINT('Ctrl Pts',(15.7480221813554,-8.60398998850506,11.6740328814034));
#17752=CARTESIAN_POINT('Ctrl Pts',(15.6946673265394,-8.65045910276734,11.7104534520236));
#17753=CARTESIAN_POINT('Ctrl Pts',(15.5889287876151,-8.72923310580083,11.792477615238));
#17754=CARTESIAN_POINT('Ctrl Pts',(15.5369709165891,-8.76172601103371,11.8373807749035));
#17755=CARTESIAN_POINT('Ctrl Pts',(15.4102920066095,-8.82316162407197,11.9600005325281));
#17756=CARTESIAN_POINT('Ctrl Pts',(15.3183831004453,-8.8528704254883,12.0602246502956));
#17757=CARTESIAN_POINT('Ctrl Pts',(15.0640351590599,-8.86324989111337,12.3877046968413));
#17758=CARTESIAN_POINT('Ctrl Pts',(14.8841363200047,-8.84858870230231,12.6363765585959));
#17759=CARTESIAN_POINT('Ctrl Pts',(14.657256909085,-8.73666657015347,13.00313230344));
#17760=CARTESIAN_POINT('Origin',(15.8,0.,0.));
#17761=CARTESIAN_POINT('Origin',(15.75,0.,0.));
#17762=CARTESIAN_POINT('',(14.657256909085,-12.3272525341113,9.66693526506972));
#17763=CARTESIAN_POINT('',(15.8,-9.9801646912522,10.4452137610133));
#17764=CARTESIAN_POINT('Ctrl Pts',(14.657256909085,-12.3272525341113,9.66693526506972));
#17765=CARTESIAN_POINT('Ctrl Pts',(14.6763724381383,-12.1696437112339,9.83487514324528));
#17766=CARTESIAN_POINT('Ctrl Pts',(14.6998065311112,-11.989130820148,10.0150998138746));
#17767=CARTESIAN_POINT('Ctrl Pts',(14.7651359522564,-11.6422840832012,10.3114964463897));
#17768=CARTESIAN_POINT('Ctrl Pts',(14.7991842945105,-11.5230333389356,10.3884212926736));
#17769=CARTESIAN_POINT('Ctrl Pts',(14.8880411294634,-11.2800254629345,10.514068828599));
#17770=CARTESIAN_POINT('Ctrl Pts',(14.9527298447854,-11.1787567277925,10.5206211879141));
#17771=CARTESIAN_POINT('Ctrl Pts',(15.1817050684299,-10.7894374125385,10.5746392914487));
#17772=CARTESIAN_POINT('Ctrl Pts',(15.2414935132389,-10.658964158777,10.6149814278134));
#17773=CARTESIAN_POINT('Ctrl Pts',(15.4262634482945,-10.390416781695,10.6030819742848));
#17774=CARTESIAN_POINT('Ctrl Pts',(15.4835457818311,-10.3135836261246,10.5926634708532));
#17775=CARTESIAN_POINT('Ctrl Pts',(15.6181084961506,-10.1496580380588,10.5516215338609));
#17776=CARTESIAN_POINT('Ctrl Pts',(15.7034661294835,-10.0585632293465,10.5127217304131));
#17777=CARTESIAN_POINT('Ctrl Pts',(15.8,-9.9801646912522,10.4452137610133));
#17778=CARTESIAN_POINT('',(15.8,-11.7322498653003,8.42973848206085));
#17779=CARTESIAN_POINT('Ctrl Pts',(15.8,-11.7322498653004,8.42973848206086));
#17780=CARTESIAN_POINT('Ctrl Pts',(15.7480221813559,-11.790355297951,8.4438859174225));
#17781=CARTESIAN_POINT('Ctrl Pts',(15.6946673265394,-11.8458046271437,8.46416419241756));
#17782=CARTESIAN_POINT('Ctrl Pts',(15.5889287876151,-11.946070016426,8.51783130168396));
#17783=CARTESIAN_POINT('Ctrl Pts',(15.5369709165889,-11.990848445119,8.55049588437264));
#17784=CARTESIAN_POINT('Ctrl Pts',(15.4102920065756,-12.0871687742093,8.64812955542542));
#17785=CARTESIAN_POINT('Ctrl Pts',(15.318383100414,-12.1463944790119,8.73426783120985));
#17786=CARTESIAN_POINT('Ctrl Pts',(15.0640351588785,-12.2574628371972,9.0425124323448));
#17787=CARTESIAN_POINT('Ctrl Pts',(14.8841363198405,-12.3203630492726,9.28354398344375));
#17788=CARTESIAN_POINT('Ctrl Pts',(14.657256909085,-12.3272525341113,9.66693526506972));
#17789=CARTESIAN_POINT('Origin',(15.8,0.,0.));
#17790=CARTESIAN_POINT('Origin',(15.75,0.,0.));
#17791=CARTESIAN_POINT('',(14.657256909085,-14.7111611310115,5.38447124945594));
#17792=CARTESIAN_POINT('',(15.8,-12.7194492253464,6.84994811524973));
#17793=CARTESIAN_POINT('Ctrl Pts',(14.657256909085,-14.7111611310115,5.38447124945595));
#17794=CARTESIAN_POINT('Ctrl Pts',(14.6763724381389,-14.6131625093749,5.59289536967964));
#17795=CARTESIAN_POINT('Ctrl Pts',(14.6998065311128,-14.4971770340571,5.8200807681381));
#17796=CARTESIAN_POINT('Ctrl Pts',(14.7651359522601,-14.2588977812484,6.20915225305788));
#17797=CARTESIAN_POINT('Ctrl Pts',(14.7991842945143,-14.1692546686343,6.31916263594739));
#17798=CARTESIAN_POINT('Ctrl Pts',(14.8880411294636,-13.9769676685657,6.51375410718182));
#17799=CARTESIAN_POINT('Ctrl Pts',(14.9527298447806,-13.8826801684986,6.55127953136504));
#17800=CARTESIAN_POINT('Ctrl Pts',(15.1817050684442,-13.5291080087754,6.72296008539242));
#17801=CARTESIAN_POINT('Ctrl Pts',(15.241493513237,-13.4174869763346,6.80164618977413));
#17802=CARTESIAN_POINT('Ctrl Pts',(15.4262634482843,-13.1584061100718,6.87331484027025));
#17803=CARTESIAN_POINT('Ctrl Pts',(15.4835457818224,-13.0821139421803,6.88714900549545));
#17804=CARTESIAN_POINT('Ctrl Pts',(15.6181084961469,-12.9135287874431,6.89877159640481));
#17805=CARTESIAN_POINT('Ctrl Pts',(15.7034661294807,-12.814871775672,6.88992552884512));
#17806=CARTESIAN_POINT('Ctrl Pts',(15.8,-12.7194492253464,6.84994811524973));
#17807=CARTESIAN_POINT('',(15.8,-13.7629651342901,4.39169312339699));
#17808=CARTESIAN_POINT('Ctrl Pts',(15.8,-13.7629651342901,4.39169312339699));
#17809=CARTESIAN_POINT('Ctrl Pts',(15.7480221813558,-13.8225984825983,4.387192567832));
#17810=CARTESIAN_POINT('Ctrl Pts',(15.6946673265393,-13.8816002600413,4.38934356835805));
#17811=CARTESIAN_POINT('Ctrl Pts',(15.5889287876154,-13.993542360679,4.40940031310068));
#17812=CARTESIAN_POINT('Ctrl Pts',(15.5369709165891,-14.046223088242,4.42662888187123));
#17813=CARTESIAN_POINT('Ctrl Pts',(15.4102920065779,-14.1679996284516,4.48971940234203));
#17814=CARTESIAN_POINT('Ctrl Pts',(15.3183831004165,-14.2509448120201,4.55334002154002));
#17815=CARTESIAN_POINT('Ctrl Pts',(15.0640351588442,-14.4518299180306,4.81217604788315));
#17816=CARTESIAN_POINT('Ctrl Pts',(14.8841363197935,-14.5861344200701,5.02197344074748));
#17817=CARTESIAN_POINT('Ctrl Pts',(14.657256909085,-14.7111611310115,5.38447124945594));
#17818=CARTESIAN_POINT('Origin',(15.8,0.,0.));
#17819=CARTESIAN_POINT('Origin',(15.75,0.,0.));
#17820=CARTESIAN_POINT('',(14.657256909085,-15.6550387777217,0.574937672128249));
#17821=CARTESIAN_POINT('',(15.8,-14.2136654476498,2.58416182157067));
#17822=CARTESIAN_POINT('Ctrl Pts',(14.657256909085,-15.6550387777217,0.574937672128249));
#17823=CARTESIAN_POINT('Ctrl Pts',(14.6763724381385,-15.6262431452137,0.803444029325674));
#17824=CARTESIAN_POINT('Ctrl Pts',(14.6998065311114,-15.5861385521163,1.05535166589991));
#17825=CARTESIAN_POINT('Ctrl Pts',(14.7651359522591,-15.4797512169005,1.49901297547856));
#17826=CARTESIAN_POINT('Ctrl Pts',(14.7991842945149,-15.4284906283764,1.63134031221159));
#17827=CARTESIAN_POINT('Ctrl Pts',(14.8880411294635,-15.3057468955348,1.87582774976688));
#17828=CARTESIAN_POINT('Ctrl Pts',(14.9527298447838,-15.2276701479809,1.94065298884041));
#17829=CARTESIAN_POINT('Ctrl Pts',(15.181705068436,-14.9444552503071,2.213190704551));
#17830=CARTESIAN_POINT('Ctrl Pts',(15.2414935132407,-14.8626126835091,2.32251843283411));
#17831=CARTESIAN_POINT('Ctrl Pts',(15.4262634482963,-14.6383589683605,2.47073976049581));
#17832=CARTESIAN_POINT('Ctrl Pts',(15.4835457818331,-14.5700757971043,2.507472409895));
#17833=CARTESIAN_POINT('Ctrl Pts',(15.618108496131,-14.4133333652819,2.57062182851381));
#17834=CARTESIAN_POINT('Ctrl Pts',(15.7034661294645,-14.316771386148,2.59269541157943));
#17835=CARTESIAN_POINT('Ctrl Pts',(15.8,-14.2136654476498,2.58416182157067));
#17836=CARTESIAN_POINT('',(15.8,-14.4464654837189,-0.0762417569101986));
#17837=CARTESIAN_POINT('Ctrl Pts',(15.8,-14.4464654837189,-0.0762417569101976));
#17838=CARTESIAN_POINT('Ctrl Pts',(15.7480221813552,-14.5017894200628,-0.0989497576662283));
#17839=CARTESIAN_POINT('Ctrl Pts',(15.6946673265391,-14.55856814069,-0.115136586527329));
#17840=CARTESIAN_POINT('Ctrl Pts',(15.5889287876155,-14.6712292799262,-0.130653500227226));
#17841=CARTESIAN_POINT('Ctrl Pts',(15.5369709165891,-14.7266555496972,-0.130547397724577));
#17842=CARTESIAN_POINT('Ctrl Pts',(15.4102920065966,-14.8619679647848,-0.108175767558644));
#17843=CARTESIAN_POINT('Ctrl Pts',(15.3183831004334,-14.9605133746397,-0.0733004344328703));
#17844=CARTESIAN_POINT('Ctrl Pts',(15.0640351589848,-15.2315511945023,0.110790343309237));
#17845=CARTESIAN_POINT('Ctrl Pts',(14.8841363199333,-15.424113326113,0.268817147256498));
#17846=CARTESIAN_POINT('Ctrl Pts',(14.657256909085,-15.6550387777217,0.574937672128249));
#17847=CARTESIAN_POINT('Origin',(15.8,0.,0.));
#17848=CARTESIAN_POINT('Origin',(15.75,0.,0.));
#17849=CARTESIAN_POINT('',(14.657256909085,-15.0664921537995,-4.29087481037367));
#17850=CARTESIAN_POINT('',(15.8,-14.3165490635069,-1.93458023611785));
#17851=CARTESIAN_POINT('Ctrl Pts',(14.657256909085,-15.0664921537995,-4.29087481037367));
#17852=CARTESIAN_POINT('Ctrl Pts',(14.6763724381386,-15.109718227559,-4.06465401053565));
#17853=CARTESIAN_POINT('Ctrl Pts',(14.6998065311121,-15.1494202336756,-3.81268261044208));
#17854=CARTESIAN_POINT('Ctrl Pts',(14.765135952259,-15.1853387496716,-3.35786013638255));
#17855=CARTESIAN_POINT('Ctrl Pts',(14.7991842945136,-15.1774784287992,-3.21616896750232));
#17856=CARTESIAN_POINT('Ctrl Pts',(14.8880411294635,-15.1362929749603,-2.94571769745994));
#17857=CARTESIAN_POINT('Ctrl Pts',(14.9527298447828,-15.0820696759676,-2.85993818955902));
#17858=CARTESIAN_POINT('Ctrl Pts',(15.1817050684391,-14.8969350877823,-2.51322120264979));
#17859=CARTESIAN_POINT('Ctrl Pts',(15.2414935132397,-14.8528823073179,-2.38395361025663));
#17860=CARTESIAN_POINT('Ctrl Pts',(15.4262634482939,-14.6854072594002,-2.17368854169763));
#17861=CARTESIAN_POINT('Ctrl Pts',(15.483545781831,-14.6318171173362,-2.11765305577722));
#17862=CARTESIAN_POINT('Ctrl Pts',(15.6181084961287,-14.5022604497099,-2.00915831452651));
#17863=CARTESIAN_POINT('Ctrl Pts',(15.7034661294625,-14.4172456625222,-1.95832579695004));
#17864=CARTESIAN_POINT('Ctrl Pts',(15.8,-14.3165490635069,-1.93458023611785));
#17865=CARTESIAN_POINT('',(15.8,-13.7158451371576,-4.53671356284346));
#17866=CARTESIAN_POINT('Ctrl Pts',(15.8,-13.7158451371576,-4.53671356284346));
#17867=CARTESIAN_POINT('Ctrl Pts',(15.7480221813554,-13.7614441691826,-4.57540619146037));
#17868=CARTESIAN_POINT('Ctrl Pts',(15.694667326539,-13.8104419362191,-4.60834637011974));
#17869=CARTESIAN_POINT('Ctrl Pts',(15.5889287876157,-13.9127940567892,-4.65791803863634));
#17870=CARTESIAN_POINT('Ctrl Pts',(15.5369709165891,-13.9655403593054,-4.67494478845391));
#17871=CARTESIAN_POINT('Ctrl Pts',(15.4102920065913,-14.101143327329,-4.69548193961731));
#17872=CARTESIAN_POINT('Ctrl Pts',(15.3183831004285,-14.2056426521431,-4.69276573315023));
#17873=CARTESIAN_POINT('Ctrl Pts',(15.0640351589399,-14.5203021157653,-4.60144029183033));
#17874=CARTESIAN_POINT('Ctrl Pts',(14.8841363198868,-14.7522725538208,-4.51065284129877));
#17875=CARTESIAN_POINT('Ctrl Pts',(14.657256909085,-15.0664921537995,-4.29087481037367));
#17876=CARTESIAN_POINT('Origin',(15.8,0.,0.));
#17877=CARTESIAN_POINT('Origin',(15.75,0.,0.));
#17878=CARTESIAN_POINT('',(14.657256909085,-13.00313230344,-8.73666657015347));
#17879=CARTESIAN_POINT('',(15.8,-13.0180291077652,-6.26395210128206));
#17880=CARTESIAN_POINT('Ctrl Pts',(14.657256909085,-13.00313230344,-8.73666657015347));
#17881=CARTESIAN_POINT('Ctrl Pts',(14.6763724381383,-13.1141488141921,-8.53487539574091));
#17882=CARTESIAN_POINT('Ctrl Pts',(14.6998065311112,-13.2297711105418,-8.30750494836842));
#17883=CARTESIAN_POINT('Ctrl Pts',(14.7651359522592,-13.404479523151,-7.88604250249817));
#17884=CARTESIAN_POINT('Ctrl Pts',(14.7991842945157,-13.4407888928998,-7.74885722030159));
#17885=CARTESIAN_POINT('Ctrl Pts',(14.8880411294636,-13.4851932372431,-7.47891577243508));
#17886=CARTESIAN_POINT('Ctrl Pts',(14.9527298447833,-13.4601311411105,-7.38057869160189));
#17887=CARTESIAN_POINT('Ctrl Pts',(15.1817050684368,-13.39119912582,-6.99362150789967));
#17888=CARTESIAN_POINT('Ctrl Pts',(15.2414935132409,-13.3892483247688,-6.85706766398949));
#17889=CARTESIAN_POINT('Ctrl Pts',(15.4262634482971,-13.2949455686362,-6.60534106444548));
#17890=CARTESIAN_POINT('Ctrl Pts',(15.4835457818346,-13.2612942322542,-6.53548788578821));
#17891=CARTESIAN_POINT('Ctrl Pts',(15.6181084961093,-13.1716052381403,-6.39226804313223));
#17892=CARTESIAN_POINT('Ctrl Pts',(15.7034661294435,-13.1064594826067,-6.31765243202665));
#17893=CARTESIAN_POINT('Ctrl Pts',(15.8,-13.0180291077652,-6.26395210128207));
#17894=CARTESIAN_POINT('',(15.8,-11.642622304659,-8.55310023610356));
#17895=CARTESIAN_POINT('Ctrl Pts',(15.8,-11.642622304659,-8.55310023610356));
#17896=CARTESIAN_POINT('Ctrl Pts',(15.748022181353,-11.6740328814048,-8.60398998850739));
#17897=CARTESIAN_POINT('Ctrl Pts',(15.6946673265384,-11.7104534520244,-8.65045910276812));
#17898=CARTESIAN_POINT('Ctrl Pts',(15.5889287876162,-11.7924776152371,-8.72923310580004));
#17899=CARTESIAN_POINT('Ctrl Pts',(15.5369709165894,-11.8373807749032,-8.76172601103358));
#17900=CARTESIAN_POINT('Ctrl Pts',(15.4102920066065,-11.960000532531,-8.82316162407342));
#17901=CARTESIAN_POINT('Ctrl Pts',(15.318383100443,-12.0602246502986,-8.85287042548839));
#17902=CARTESIAN_POINT('Ctrl Pts',(15.0640351590301,-12.3877046968796,-8.8632498911146));
#17903=CARTESIAN_POINT('Ctrl Pts',(14.8841363199762,-12.6363765586419,-8.84858870228826));
#17904=CARTESIAN_POINT('Ctrl Pts',(14.657256909085,-13.00313230344,-8.73666657015347));
#17905=CARTESIAN_POINT('Origin',(15.8,0.,0.));
#17906=CARTESIAN_POINT('Origin',(15.75,0.,0.));
#17907=CARTESIAN_POINT('',(14.657256909085,-9.66693526506972,-12.3272525341113));
#17908=CARTESIAN_POINT('',(15.8,-10.4452137610133,-9.9801646912522));
#17909=CARTESIAN_POINT('Ctrl Pts',(14.657256909085,-9.66693526506972,-12.3272525341113));
#17910=CARTESIAN_POINT('Ctrl Pts',(14.6763724381384,-9.83487514324582,-12.1696437112334));
#17911=CARTESIAN_POINT('Ctrl Pts',(14.6998065311114,-10.015099813876,-11.9891308201465));
#17912=CARTESIAN_POINT('Ctrl Pts',(14.7651359522567,-10.3114964463902,-11.6422840832003));
#17913=CARTESIAN_POINT('Ctrl Pts',(14.7991842945106,-10.3884212926739,-11.523033338935));
#17914=CARTESIAN_POINT('Ctrl Pts',(14.8880411294633,-10.5140688285986,-11.2800254629351));
#17915=CARTESIAN_POINT('Ctrl Pts',(14.9527298447848,-10.5206211879141,-11.1787567277935));
#17916=CARTESIAN_POINT('Ctrl Pts',(15.1817050684351,-10.5746392914498,-10.7894374125298));
#17917=CARTESIAN_POINT('Ctrl Pts',(15.2414935132425,-10.6149814278149,-10.6589641587703));
#17918=CARTESIAN_POINT('Ctrl Pts',(15.4262634483023,-10.6030819742836,-10.3904167816842));
#17919=CARTESIAN_POINT('Ctrl Pts',(15.4835457818389,-10.5926634708515,-10.3135836261144));
#17920=CARTESIAN_POINT('Ctrl Pts',(15.6181084961081,-10.551621533873,-10.1496580381114));
#17921=CARTESIAN_POINT('Ctrl Pts',(15.703466129442,-10.5127217304422,-10.0585632293802));
#17922=CARTESIAN_POINT('Ctrl Pts',(15.8,-10.4452137610133,-9.98016469125221));
#17923=CARTESIAN_POINT('',(15.8,-8.42973848206085,-11.7322498653004));
#17924=CARTESIAN_POINT('Ctrl Pts',(15.8,-8.42973848206086,-11.7322498653004));
#17925=CARTESIAN_POINT('Ctrl Pts',(15.7480221813553,-8.44388591742267,-11.7903552979517));
#17926=CARTESIAN_POINT('Ctrl Pts',(15.6946673265394,-8.46416419241757,-11.8458046271437));
#17927=CARTESIAN_POINT('Ctrl Pts',(15.5889287876151,-8.51783130168398,-11.946070016426));
#17928=CARTESIAN_POINT('Ctrl Pts',(15.536970916589,-8.55049588437258,-11.9908484451189));
#17929=CARTESIAN_POINT('Ctrl Pts',(15.4102920065769,-8.64812955542444,-12.0871687742084));
#17930=CARTESIAN_POINT('Ctrl Pts',(15.3183831004154,-8.73426783120814,-12.1463944790113));
#17931=CARTESIAN_POINT('Ctrl Pts',(15.0640351588785,-9.04251243234484,-12.2574628371973));
#17932=CARTESIAN_POINT('Ctrl Pts',(14.8841363198405,-9.28354398344382,-12.3203630492726));
#17933=CARTESIAN_POINT('Ctrl Pts',(14.657256909085,-9.66693526506972,-12.3272525341113));
#17934=CARTESIAN_POINT('Origin',(15.8,0.,0.));
#17935=CARTESIAN_POINT('Origin',(15.75,0.,0.));
#17936=CARTESIAN_POINT('',(14.657256909085,-5.38447124945594,-14.7111611310115));
#17937=CARTESIAN_POINT('',(15.8,-6.84994811524973,-12.7194492253464));
#17938=CARTESIAN_POINT('Ctrl Pts',(14.657256909085,-5.38447124945595,-14.7111611310115));
#17939=CARTESIAN_POINT('Ctrl Pts',(14.6763724381384,-5.59289536967403,-14.6131625093775));
#17940=CARTESIAN_POINT('Ctrl Pts',(14.6998065311115,-5.82008076812493,-14.4971770340638));
#17941=CARTESIAN_POINT('Ctrl Pts',(14.7651359522571,-6.20915225304582,-14.2588977812571));
#17942=CARTESIAN_POINT('Ctrl Pts',(14.7991842945112,-6.31916263593875,-14.1692546686417));
#17943=CARTESIAN_POINT('Ctrl Pts',(14.8880411294635,-6.51375410718485,-13.9769676685645));
#17944=CARTESIAN_POINT('Ctrl Pts',(14.952729844784,-6.55127953136673,-13.8826801684939));
#17945=CARTESIAN_POINT('Ctrl Pts',(15.181705068435,-6.72296008538707,-13.5291080087886));
#17946=CARTESIAN_POINT('Ctrl Pts',(15.2414935132397,-6.80164618977864,-13.4174869763291));
#17947=CARTESIAN_POINT('Ctrl Pts',(15.4262634482948,-6.87331484027296,-13.1584061100578));
#17948=CARTESIAN_POINT('Ctrl Pts',(15.4835457818317,-6.88714900549704,-13.0821139421683));
#17949=CARTESIAN_POINT('Ctrl Pts',(15.618108496136,-6.8987715964028,-12.9135287874573));
#17950=CARTESIAN_POINT('Ctrl Pts',(15.7034661294695,-6.88992552884981,-12.8148717756832));
#17951=CARTESIAN_POINT('Ctrl Pts',(15.8,-6.84994811524973,-12.7194492253464));
#17952=CARTESIAN_POINT('',(15.8,-4.391693123397,-13.7629651342901));
#17953=CARTESIAN_POINT('Ctrl Pts',(15.8,-4.391693123397,-13.7629651342901));
#17954=CARTESIAN_POINT('Ctrl Pts',(15.7480221813555,-4.38719256783197,-13.8225984825987));
#17955=CARTESIAN_POINT('Ctrl Pts',(15.6946673265391,-4.38934356835812,-13.8816002600416));
#17956=CARTESIAN_POINT('Ctrl Pts',(15.5889287876154,-4.40940031310067,-13.993542360679));
#17957=CARTESIAN_POINT('Ctrl Pts',(15.5369709165889,-4.42662888187134,-14.0462230882423));
#17958=CARTESIAN_POINT('Ctrl Pts',(15.4102920065966,-4.48971940233274,-14.1679996284337));
#17959=CARTESIAN_POINT('Ctrl Pts',(15.3183831004327,-4.55334002152343,-14.2509448120073));
#17960=CARTESIAN_POINT('Ctrl Pts',(15.0640351589831,-4.81217604774183,-14.4518299179208));
#17961=CARTESIAN_POINT('Ctrl Pts',(14.8841363199243,-5.02197344053858,-14.586134419998));
#17962=CARTESIAN_POINT('Ctrl Pts',(14.657256909085,-5.38447124945595,-14.7111611310115));
#17963=CARTESIAN_POINT('Origin',(15.8,0.,0.));
#17964=CARTESIAN_POINT('Origin',(15.75,0.,0.));
#17965=CARTESIAN_POINT('',(14.657256909085,-0.57493767212825,-15.6550387777217));
#17966=CARTESIAN_POINT('',(15.8,-2.58416182157067,-14.2136654476498));
#17967=CARTESIAN_POINT('Ctrl Pts',(14.657256909085,-0.57493767212825,-15.6550387777217));
#17968=CARTESIAN_POINT('Ctrl Pts',(14.6763724381382,-0.803444029322114,
-15.6262431452141));
#17969=CARTESIAN_POINT('Ctrl Pts',(14.6998065311109,-1.05535166589373,-15.5861385521174));
#17970=CARTESIAN_POINT('Ctrl Pts',(14.7651359522566,-1.49901297546359,-15.4797512169046));
#17971=CARTESIAN_POINT('Ctrl Pts',(14.7991842945114,-1.63134031220087,-15.4284906283814));
#17972=CARTESIAN_POINT('Ctrl Pts',(14.8880411294633,-1.87582774976806,-15.3057468955348));
#17973=CARTESIAN_POINT('Ctrl Pts',(14.9527298447852,-1.94065298884167,-15.2276701479793));
#17974=CARTESIAN_POINT('Ctrl Pts',(15.1817050684308,-2.21319070454549,-14.9444552503134));
#17975=CARTESIAN_POINT('Ctrl Pts',(15.24149351324,-2.3225184328336,-14.8626126835099));
#17976=CARTESIAN_POINT('Ctrl Pts',(15.4262634482958,-2.47073976049543,-14.6383589683611));
#17977=CARTESIAN_POINT('Ctrl Pts',(15.483545781833,-2.507472409895,-14.5700757971044));
#17978=CARTESIAN_POINT('Ctrl Pts',(15.6181084961295,-2.57062182851311,-14.4133333652836));
#17979=CARTESIAN_POINT('Ctrl Pts',(15.7034661294631,-2.59269541157956,-14.3167713861495));
#17980=CARTESIAN_POINT('Ctrl Pts',(15.8,-2.58416182157067,-14.2136654476498));
#17981=CARTESIAN_POINT('',(15.8,0.0762417569101962,-14.4464654837189));
#17982=CARTESIAN_POINT('Ctrl Pts',(15.8,0.0762417569101968,-14.4464654837189));
#17983=CARTESIAN_POINT('Ctrl Pts',(15.7480221813555,0.0989497576660791,
-14.5017894200625));
#17984=CARTESIAN_POINT('Ctrl Pts',(15.6946673265393,0.115136586527307,-14.5585681406898));
#17985=CARTESIAN_POINT('Ctrl Pts',(15.5889287876154,0.130653500227241,-14.6712292799264));
#17986=CARTESIAN_POINT('Ctrl Pts',(15.5369709165891,0.130547397724574,-14.7266555496972));
#17987=CARTESIAN_POINT('Ctrl Pts',(15.410292006597,0.108175767558706,-14.8619679647844));
#17988=CARTESIAN_POINT('Ctrl Pts',(15.3183831004337,0.0733004344331047,
-14.9605133746394));
#17989=CARTESIAN_POINT('Ctrl Pts',(15.0640351589872,-0.110790343307477,
-15.2315511944997));
#17990=CARTESIAN_POINT('Ctrl Pts',(14.8841363199356,-0.268817147253357,
-15.4241133261106));
#17991=CARTESIAN_POINT('Ctrl Pts',(14.657256909085,-0.57493767212825,-15.6550387777217));
#17992=CARTESIAN_POINT('Origin',(15.8,0.,0.));
#17993=CARTESIAN_POINT('Origin',(15.75,0.,0.));
#17994=CARTESIAN_POINT('',(14.657256909085,4.29087481037367,-15.0664921537995));
#17995=CARTESIAN_POINT('',(15.8,1.93458023611785,-14.3165490635069));
#17996=CARTESIAN_POINT('Ctrl Pts',(14.657256909085,4.29087481037367,-15.0664921537995));
#17997=CARTESIAN_POINT('Ctrl Pts',(14.6763724381383,4.06465401053917,-15.1097182275583));
#17998=CARTESIAN_POINT('Ctrl Pts',(14.6998065311113,3.81268261045103,-15.1494202336741));
#17999=CARTESIAN_POINT('Ctrl Pts',(14.7651359522575,3.35786013638889,-15.1853387496718));
#18000=CARTESIAN_POINT('Ctrl Pts',(14.7991842945124,3.216168967507,-15.1774784287995));
#18001=CARTESIAN_POINT('Ctrl Pts',(14.8880411294634,2.94571769745822,-15.1362929749609));
#18002=CARTESIAN_POINT('Ctrl Pts',(14.9527298447845,2.85993818955692,-15.0820696759661));
#18003=CARTESIAN_POINT('Ctrl Pts',(15.1817050684319,2.51322120265964,-14.8969350877882));
#18004=CARTESIAN_POINT('Ctrl Pts',(15.2414935132387,2.38395361025797,-14.8528823073188));
#18005=CARTESIAN_POINT('Ctrl Pts',(15.4262634482925,2.17368854169906,-14.6854072594014));
#18006=CARTESIAN_POINT('Ctrl Pts',(15.4835457818303,2.11765305577787,-14.6318171173369));
#18007=CARTESIAN_POINT('Ctrl Pts',(15.6181084961299,2.00915831452544,-14.5022604497087));
#18008=CARTESIAN_POINT('Ctrl Pts',(15.7034661294637,1.95832579694974,-14.4172456625209));
#18009=CARTESIAN_POINT('Ctrl Pts',(15.8,1.93458023611785,-14.3165490635069));
#18010=CARTESIAN_POINT('',(15.8,4.53671356284346,-13.7158451371576));
#18011=CARTESIAN_POINT('Ctrl Pts',(15.8,4.53671356284346,-13.7158451371576));
#18012=CARTESIAN_POINT('Ctrl Pts',(15.7480221813544,4.57540619146115,-13.7614441691835));
#18013=CARTESIAN_POINT('Ctrl Pts',(15.694667326539,4.60834637011977,-13.8104419362192));
#18014=CARTESIAN_POINT('Ctrl Pts',(15.5889287876155,4.65791803863639,-13.9127940567893));
#18015=CARTESIAN_POINT('Ctrl Pts',(15.5369709165891,4.67494478845389,-13.9655403593054));
#18016=CARTESIAN_POINT('Ctrl Pts',(15.4102920066053,4.69548193961504,-14.101143327314));
#18017=CARTESIAN_POINT('Ctrl Pts',(15.3183831004414,4.69276573315488,-14.2056426521272));
#18018=CARTESIAN_POINT('Ctrl Pts',(15.0640351590345,4.60144029186426,-14.5203021156484));
#18019=CARTESIAN_POINT('Ctrl Pts',(14.8841363199801,4.51065284138912,-14.7522725536916));
#18020=CARTESIAN_POINT('Ctrl Pts',(14.657256909085,4.29087481037367,-15.0664921537995));
#18021=CARTESIAN_POINT('Origin',(15.8,0.,0.));
#18022=CARTESIAN_POINT('Origin',(15.75,0.,0.));
#18023=CARTESIAN_POINT('',(14.657256909085,8.73666657015347,-13.00313230344));
#18024=CARTESIAN_POINT('',(15.8,6.26395210128206,-13.0180291077652));
#18025=CARTESIAN_POINT('Ctrl Pts',(14.657256909085,8.73666657015347,-13.00313230344));
#18026=CARTESIAN_POINT('Ctrl Pts',(14.6763724381385,8.53487539573899,-13.1141488141932));
#18027=CARTESIAN_POINT('Ctrl Pts',(14.6998065311118,8.30750494836237,-13.229771110545));
#18028=CARTESIAN_POINT('Ctrl Pts',(14.7651359522573,7.88604250251314,-13.4044795231442));
#18029=CARTESIAN_POINT('Ctrl Pts',(14.7991842945111,7.74885722031548,-13.4407888928976));
#18030=CARTESIAN_POINT('Ctrl Pts',(14.8880411294636,7.47891577243524,-13.4851932372429));
#18031=CARTESIAN_POINT('Ctrl Pts',(14.9527298447839,7.3805786916008,-13.4601311411104));
#18032=CARTESIAN_POINT('Ctrl Pts',(15.181705068435,6.99362150790287,-13.3911991258204));
#18033=CARTESIAN_POINT('Ctrl Pts',(15.2414935132393,6.85706766399212,-13.3892483247693));
#18034=CARTESIAN_POINT('Ctrl Pts',(15.4262634482953,6.60534106444771,-13.2949455686372));
#18035=CARTESIAN_POINT('Ctrl Pts',(15.4835457818325,6.53548788579067,-13.2612942322554));
#18036=CARTESIAN_POINT('Ctrl Pts',(15.6181084961243,6.39226804311592,-13.1716052381305));
#18037=CARTESIAN_POINT('Ctrl Pts',(15.7034661294581,6.31765243201851,-13.1064594825933));
#18038=CARTESIAN_POINT('Ctrl Pts',(15.8,6.26395210128206,-13.0180291077652));
#18039=CARTESIAN_POINT('',(15.8,8.55310023610356,-11.642622304659));
#18040=CARTESIAN_POINT('Ctrl Pts',(15.8,8.55310023610356,-11.642622304659));
#18041=CARTESIAN_POINT('Ctrl Pts',(15.7480221813542,8.60398998850618,-11.6740328814041));
#18042=CARTESIAN_POINT('Ctrl Pts',(15.694667326539,8.65045910276766,-11.7104534520239));
#18043=CARTESIAN_POINT('Ctrl Pts',(15.5889287876153,8.72923310580071,-11.7924776152379));
#18044=CARTESIAN_POINT('Ctrl Pts',(15.5369709165891,8.76172601103374,-11.8373807749035));
#18045=CARTESIAN_POINT('Ctrl Pts',(15.4102920066146,8.82316162406948,-11.9600005325232));
#18046=CARTESIAN_POINT('Ctrl Pts',(15.3183831004499,8.85287042548813,-12.0602246502897));
#18047=CARTESIAN_POINT('Ctrl Pts',(15.0640351591031,8.8632498911116,-12.3877046967857));
#18048=CARTESIAN_POINT('Ctrl Pts',(14.884136320048,8.84858870232365,-12.6363765585259));
#18049=CARTESIAN_POINT('Ctrl Pts',(14.657256909085,8.73666657015347,-13.00313230344));
#18050=CARTESIAN_POINT('Origin',(15.8,0.,0.));
#18051=CARTESIAN_POINT('Origin',(15.75,0.,0.));
#18052=CARTESIAN_POINT('',(14.657256909085,12.3272525341113,-9.66693526506972));
#18053=CARTESIAN_POINT('',(15.8,9.9801646912522,-10.4452137610133));
#18054=CARTESIAN_POINT('Ctrl Pts',(14.657256909085,12.3272525341113,-9.66693526506972));
#18055=CARTESIAN_POINT('Ctrl Pts',(14.6763724381382,12.1696437112347,-9.83487514324446));
#18056=CARTESIAN_POINT('Ctrl Pts',(14.699806531111,11.9891308201493,-10.0150998138733));
#18057=CARTESIAN_POINT('Ctrl Pts',(14.7651359522566,11.6422840831999,-10.311496446391));
#18058=CARTESIAN_POINT('Ctrl Pts',(14.7991842945111,11.5230333389337,-10.3884212926745));
#18059=CARTESIAN_POINT('Ctrl Pts',(14.8880411294632,11.2800254629352,-10.5140688285987));
#18060=CARTESIAN_POINT('Ctrl Pts',(14.9527298447846,11.1787567277939,-10.520621187914));
#18061=CARTESIAN_POINT('Ctrl Pts',(15.1817050684329,10.7894374125334,-10.5746392914494));
#18062=CARTESIAN_POINT('Ctrl Pts',(15.2414935132398,10.6589641587761,-10.614981427813));
#18063=CARTESIAN_POINT('Ctrl Pts',(15.4262634482933,10.3904167816966,-10.603081974285));
#18064=CARTESIAN_POINT('Ctrl Pts',(15.483545781831,10.3135836261245,-10.5926634708533));
#18065=CARTESIAN_POINT('Ctrl Pts',(15.6181084961289,10.1496580380854,-10.5516215338674));
#18066=CARTESIAN_POINT('Ctrl Pts',(15.7034661294626,10.0585632293635,-10.5127217304277));
#18067=CARTESIAN_POINT('Ctrl Pts',(15.8,9.98016469125221,-10.4452137610133));
#18068=CARTESIAN_POINT('',(15.8,11.7322498653004,-8.42973848206085));
#18069=CARTESIAN_POINT('Ctrl Pts',(15.8,11.7322498653004,-8.42973848206086));
#18070=CARTESIAN_POINT('Ctrl Pts',(15.7480221813556,11.7903552979513,-8.44388591742258));
#18071=CARTESIAN_POINT('Ctrl Pts',(15.6946673265392,11.8458046271439,-8.46416419241769));
#18072=CARTESIAN_POINT('Ctrl Pts',(15.5889287876152,11.9460700164259,-8.51783130168395));
#18073=CARTESIAN_POINT('Ctrl Pts',(15.5369709165888,11.9908484451191,-8.55049588437278));
#18074=CARTESIAN_POINT('Ctrl Pts',(15.4102920065736,12.0871687742109,-8.64812955542696));
#18075=CARTESIAN_POINT('Ctrl Pts',(15.3183831004117,12.1463944790129,-8.73426783121256));
#18076=CARTESIAN_POINT('Ctrl Pts',(15.0640351588785,12.2574628371973,-9.04251243234485));
#18077=CARTESIAN_POINT('Ctrl Pts',(14.8841363198405,12.3203630492726,-9.28354398344382));
#18078=CARTESIAN_POINT('Ctrl Pts',(14.657256909085,12.3272525341113,-9.66693526506972));
#18079=CARTESIAN_POINT('Origin',(15.8,0.,0.));
#18080=CARTESIAN_POINT('Origin',(15.75,0.,0.));
#18081=CARTESIAN_POINT('',(15.8218384638272,-14.4233723052509,1.76635367265361E-15));
#18082=CARTESIAN_POINT('Origin',(15.8218384638272,0.,0.));
#18083=CARTESIAN_POINT('',(19.5,-10.5,-1.28587913910472E-15));
#18084=CARTESIAN_POINT('',(15.75,-14.5,-1.77573785876366E-15));
#18085=CARTESIAN_POINT('Origin',(19.5,0.,0.));
#18086=CARTESIAN_POINT('Origin',(21.25,0.,0.));
#18087=CARTESIAN_POINT('',(21.,-10.5,-1.28587913910472E-15));
#18088=CARTESIAN_POINT('',(21.25,-10.5,-1.28587913910472E-15));
#18089=CARTESIAN_POINT('Origin',(21.,0.,0.));
#18090=CARTESIAN_POINT('Origin',(15.75,0.,0.));
#18091=CARTESIAN_POINT('',(14.657256909085,14.7111611310115,-5.38447124945595));
#18092=CARTESIAN_POINT('',(15.8,12.7194492253464,-6.84994811524973));
#18093=CARTESIAN_POINT('Ctrl Pts',(14.657256909085,14.7111611310115,-5.38447124945595));
#18094=CARTESIAN_POINT('Ctrl Pts',(14.6763724381386,14.6131625093767,-5.59289536967573));
#18095=CARTESIAN_POINT('Ctrl Pts',(14.6998065311119,14.4971770340621,-5.82008076812812));
#18096=CARTESIAN_POINT('Ctrl Pts',(14.7651359522581,14.258897781254,-6.20915225305041));
#18097=CARTESIAN_POINT('Ctrl Pts',(14.7991842945124,14.169254668639,-6.3191626359417));
#18098=CARTESIAN_POINT('Ctrl Pts',(14.8880411294633,13.9769676685652,-6.51375410718384));
#18099=CARTESIAN_POINT('Ctrl Pts',(14.9527298447829,13.8826801684955,-6.55127953136609));
#18100=CARTESIAN_POINT('Ctrl Pts',(15.1817050684388,13.5291080087829,-6.72296008538962));
#18101=CARTESIAN_POINT('Ctrl Pts',(15.2414935132397,13.4174869763298,-6.80164618977748));
#18102=CARTESIAN_POINT('Ctrl Pts',(15.4262634482914,13.1584061100624,-6.87331484027209));
#18103=CARTESIAN_POINT('Ctrl Pts',(15.4835457818292,13.0821139421714,-6.88714900549669));
#18104=CARTESIAN_POINT('Ctrl Pts',(15.6181084961279,12.9135287874673,-6.89877159640229));
#18105=CARTESIAN_POINT('Ctrl Pts',(15.7034661294619,12.8148717756907,-6.88992552885296));
#18106=CARTESIAN_POINT('Ctrl Pts',(15.8,12.7194492253464,-6.84994811524973));
#18107=CARTESIAN_POINT('',(15.8,13.7629651342901,-4.391693123397));
#18108=CARTESIAN_POINT('Ctrl Pts',(15.8,13.7629651342901,-4.391693123397));
#18109=CARTESIAN_POINT('Ctrl Pts',(15.7480221813554,13.8225984825988,-4.38719256783196));
#18110=CARTESIAN_POINT('Ctrl Pts',(15.694667326539,13.8816002600417,-4.38934356835814));
#18111=CARTESIAN_POINT('Ctrl Pts',(15.5889287876158,13.9935423606786,-4.4094003131006));
#18112=CARTESIAN_POINT('Ctrl Pts',(15.5369709165891,14.046223088242,-4.42662888187122));
#18113=CARTESIAN_POINT('Ctrl Pts',(15.4102920065917,14.1679996284383,-4.48971940233513));
#18114=CARTESIAN_POINT('Ctrl Pts',(15.3183831004289,14.2509448120103,-4.55334002152732));
#18115=CARTESIAN_POINT('Ctrl Pts',(15.064035158936,14.4518299179581,-4.81217604778975));
#18116=CARTESIAN_POINT('Ctrl Pts',(14.8841363198809,14.5861344200219,-5.0219734406079));
#18117=CARTESIAN_POINT('Ctrl Pts',(14.657256909085,14.7111611310115,-5.38447124945595));
#18118=CARTESIAN_POINT('Origin',(15.8,0.,0.));
#18119=CARTESIAN_POINT('Ctrl Pts',(10.0502525316942,9.07904823952839,-1.22955082275859));
#18120=CARTESIAN_POINT('Ctrl Pts',(11.9668350211294,10.626255672559,-2.28040731262864));
#18121=CARTESIAN_POINT('Ctrl Pts',(13.8834175105647,12.1734631055895,-3.33126380249869));
#18122=CARTESIAN_POINT('Ctrl Pts',(15.8,13.7206705386201,-4.38212029236875));
#18123=CARTESIAN_POINT('Ctrl Pts',(10.0502525316942,9.23541522932356,-1.23556639107773));
#18124=CARTESIAN_POINT('Ctrl Pts',(11.9668350211294,10.8110857311875,-2.30170134729121));
#18125=CARTESIAN_POINT('Ctrl Pts',(13.8834175105647,12.3868775190731,-3.36825415935173));
#18126=CARTESIAN_POINT('Ctrl Pts',(15.8,13.962548020937,-4.43438911556521));
#18127=CARTESIAN_POINT('Ctrl Pts',(10.0502525316942,9.54242006948555,-1.29909254545997));
#18128=CARTESIAN_POINT('Ctrl Pts',(11.9668350211294,11.1694737466003,-2.40552260970753));
#18129=CARTESIAN_POINT('Ctrl Pts',(13.8834175105647,12.7961532691502,-3.51235208206864));
#18130=CARTESIAN_POINT('Ctrl Pts',(15.8,14.4232069462649,-4.6187821463162));
#18131=CARTESIAN_POINT('Ctrl Pts',(10.0502525316941,10.0380523375239,-1.61547231497529));
#18132=CARTESIAN_POINT('Ctrl Pts',(11.9668350211294,11.7265860195463,-2.82582698043838));
#18133=CARTESIAN_POINT('Ctrl Pts',(13.8834175105647,13.4155069687334,-4.03604403376329));
#18134=CARTESIAN_POINT('Ctrl Pts',(15.8,15.1040406507558,-5.24639869922638));
#18135=CARTESIAN_POINT('Ctrl Pts',(10.0502525316942,10.3628708264469,-1.92675755961641));
#18136=CARTESIAN_POINT('Ctrl Pts',(11.9668350211294,12.0820376211579,-3.22250341643877));
#18137=CARTESIAN_POINT('Ctrl Pts',(13.8834175105647,13.8004759242586,-4.51903745819411));
#18138=CARTESIAN_POINT('Ctrl Pts',(15.8,15.5196427189696,-5.81478331501647));
#18139=CARTESIAN_POINT('Ctrl Pts',(10.0502525316942,10.5463163022605,-2.13832987737225));
#18140=CARTESIAN_POINT('Ctrl Pts',(11.9668350211294,12.2789538289737,-3.48877307262933));
#18141=CARTESIAN_POINT('Ctrl Pts',(13.8834175105647,14.0115913556869,-4.8392162678864));
#18142=CARTESIAN_POINT('Ctrl Pts',(15.8,15.7442288824001,-6.18965946314348));
#18143=CARTESIAN_POINT('',(10.0502525316942,10.5463163022605,-2.13832987737225));
#18144=CARTESIAN_POINT('',(15.8,13.7206705386201,-4.38212029236875));
#18145=CARTESIAN_POINT('Ctrl Pts',(15.8,13.7206705386201,-4.38212029236875));
#18146=CARTESIAN_POINT('Ctrl Pts',(15.548617912719,13.5237121602493,-4.24557960414941));
#18147=CARTESIAN_POINT('Ctrl Pts',(15.2955018759958,13.3249640154793,-4.1079402696292));
#18148=CARTESIAN_POINT('Ctrl Pts',(15.0417466762032,13.1251225182505,-3.96976145165633));
#18149=CARTESIAN_POINT('Ctrl Pts',(14.7869012710152,12.9244224444144,-3.8309889776992));
#18150=CARTESIAN_POINT('Ctrl Pts',(14.531411198903,12.7226197192327,-3.69167215691655));
#18151=CARTESIAN_POINT('Ctrl Pts',(14.2763854175014,12.5204677360886,-3.55239975640987));
#18152=CARTESIAN_POINT('Ctrl Pts',(14.0169028604353,12.3147829883978,-3.41069346140857));
#18153=CARTESIAN_POINT('Ctrl Pts',(13.7579009635647,12.1087368195378,-3.26903291905456));
#18154=CARTESIAN_POINT('Ctrl Pts',(13.5005478461954,11.9031704882056,-3.12806496166618));
#18155=CARTESIAN_POINT('Ctrl Pts',(13.309996810501,11.7509637547505,-3.02368856803761));
#18156=CARTESIAN_POINT('Ctrl Pts',(13.1203496871979,11.5990211190179,-2.91969243162131));
#18157=CARTESIAN_POINT('Ctrl Pts',(12.9320806449423,11.4476993942222,-2.81634921885376));
#18158=CARTESIAN_POINT('Ctrl Pts',(12.7398362813705,11.2931824947395,-2.71082390290202));
#18159=CARTESIAN_POINT('Ctrl Pts',(12.5465414849355,11.1373617066507,-2.60462118886898));
#18160=CARTESIAN_POINT('Ctrl Pts',(12.3528698198642,10.980602615666,-2.49810765644039));
#18161=CARTESIAN_POINT('Ctrl Pts',(12.1588877119196,10.8235922502235,-2.39142338986208));
#18162=CARTESIAN_POINT('Ctrl Pts',(11.9645275261794,10.6656407015684,-2.28442707498219));
#18163=CARTESIAN_POINT('Ctrl Pts',(11.7704660711024,10.5071588397368,-2.1775164013726));
#18164=CARTESIAN_POINT('Ctrl Pts',(11.5758128991793,10.3481937475419,-2.07027974418958));
#18165=CARTESIAN_POINT('Ctrl Pts',(11.3814602824284,10.188695283085,-1.96312905478021));
#18166=CARTESIAN_POINT('Ctrl Pts',(11.1880912392173,10.0291195021211,-1.85649845736384));
#18167=CARTESIAN_POINT('Ctrl Pts',(10.9918630490256,9.86718424000789,-1.7482912241759));
#18168=CARTESIAN_POINT('Ctrl Pts',(10.7966477335655,9.705169511719,-1.64061939633804));
#18169=CARTESIAN_POINT('Ctrl Pts',(10.6031590586335,9.54359206502118,-1.5339733721044));
#18170=CARTESIAN_POINT('Ctrl Pts',(10.4170476660414,9.38817519823576,-1.43139351779768));
#18171=CARTESIAN_POINT('Ctrl Pts',(10.2325337582959,9.23316336539109,-1.32976299718727));
#18172=CARTESIAN_POINT('Ctrl Pts',(10.0502525316942,9.07904823952839,-1.22955082275859));
#18173=CARTESIAN_POINT('Ctrl Pts',(15.8,13.7206705386201,-4.38212029236875));
#18174=CARTESIAN_POINT('Ctrl Pts',(15.8,13.7291554381927,-4.38395384756931));
#18175=CARTESIAN_POINT('Ctrl Pts',(15.8,13.7376273491274,-4.38582790366735));
#18176=CARTESIAN_POINT('Ctrl Pts',(15.8,13.7460862714518,-4.38774246062322));
#18177=CARTESIAN_POINT('Ctrl Pts',(15.8,13.7545322021969,-4.38969752766812));
#18178=CARTESIAN_POINT('Ctrl Pts',(15.8,13.7629651342901,-4.391693123397));
#18179=CARTESIAN_POINT('Ctrl Pts',(10.0502525316942,8.25473589028142,-3.97495252086484));
#18180=CARTESIAN_POINT('Ctrl Pts',(11.9668350211294,9.40148508750639,-5.45248982387649));
#18181=CARTESIAN_POINT('Ctrl Pts',(13.8834175105647,10.5482342847314,-6.93002712688815));
#18182=CARTESIAN_POINT('Ctrl Pts',(15.8,11.6949834819563,-8.4075644298998));
#18183=CARTESIAN_POINT('Ctrl Pts',(10.0502525316942,8.40159082201817,-4.02899372351995));
#18184=CARTESIAN_POINT('Ctrl Pts',(11.9668350211294,9.57068870058278,-5.52985728348808));
#18185=CARTESIAN_POINT('Ctrl Pts',(13.8834175105647,10.7397728044506,-7.03115572742428));
#18186=CARTESIAN_POINT('Ctrl Pts',(15.8,11.9088706830152,-8.53201928739242));
#18187=CARTESIAN_POINT('Ctrl Pts',(10.0502525316942,8.67393758705161,-4.18428628311195));
#18188=CARTESIAN_POINT('Ctrl Pts',(11.9668350211294,9.87945189609368,-5.73935104252815));
#18189=CARTESIAN_POINT('Ctrl Pts',(13.8834175105647,11.0844841840221,-7.29468404041884));
#18190=CARTESIAN_POINT('Ctrl Pts',(15.8,12.2899984930642,-8.84974879983504));
#18191=CARTESIAN_POINT('Ctrl Pts',(10.0502525316941,9.04754461221301,-4.63834053369693));
#18192=CARTESIAN_POINT('Ctrl Pts',(11.9668350211294,10.2794154126352,-6.31124182863328));
#18193=CARTESIAN_POINT('Ctrl Pts',(13.8834175105647,11.5116939035746,-7.98413616433455));
#18194=CARTESIAN_POINT('Ctrl Pts',(15.8,12.7435647039968,-9.6570374592709));
#18195=CARTESIAN_POINT('Ctrl Pts',(10.0502525316942,9.26027499705532,-5.0347585282786));
#18196=CARTESIAN_POINT('Ctrl Pts',(11.9668350211294,10.4948922896145,-6.79833782460276));
#18197=CARTESIAN_POINT('Ctrl Pts',(13.8834175105647,11.7285731829415,-8.56244161305559));
#18198=CARTESIAN_POINT('Ctrl Pts',(15.8,12.9631904755006,-10.3260209093797));
#18199=CARTESIAN_POINT('Ctrl Pts',(10.0502525316942,9.36936257048691,-5.29266352931554));
#18200=CARTESIAN_POINT('Ctrl Pts',(11.9668350211294,10.5998888833726,-7.11242577089739));
#18201=CARTESIAN_POINT('Ctrl Pts',(13.8834175105647,11.8304151962582,-8.93218801247923));
#18202=CARTESIAN_POINT('Ctrl Pts',(15.8,13.0609415091439,-10.7519502540611));
#18203=CARTESIAN_POINT('',(10.0502525316942,9.36936257048691,-5.29266352931554));
#18204=CARTESIAN_POINT('',(15.8,11.6949834819563,-8.4075644298998));
#18205=CARTESIAN_POINT('Ctrl Pts',(15.8,11.6949834819563,-8.4075644298998));
#18206=CARTESIAN_POINT('Ctrl Pts',(15.5486176029459,11.5498581470164,-8.21684279750606));
#18207=CARTESIAN_POINT('Ctrl Pts',(15.295501252176,11.4033701387254,-8.02452322133575));
#18208=CARTESIAN_POINT('Ctrl Pts',(15.0417457381106,11.256008997669,-7.83135270226724));
#18209=CARTESIAN_POINT('Ctrl Pts',(14.7869002270792,11.1080148725482,-7.63735242672831));
#18210=CARTESIAN_POINT('Ctrl Pts',(14.5314100499567,10.9591402752373,-7.44249371079193));
#18211=CARTESIAN_POINT('Ctrl Pts',(14.2763841657392,10.8099197880111,-7.24756931575073));
#18212=CARTESIAN_POINT('Ctrl Pts',(14.0169020050303,10.658091848795,-7.04923884684408));
#18213=CARTESIAN_POINT('Ctrl Pts',(13.7579005049326,10.505906041498,-6.85084020761633));
#18214=CARTESIAN_POINT('Ctrl Pts',(13.5005477794198,10.3539625665122,-6.65324852970488));
#18215=CARTESIAN_POINT('Ctrl Pts',(13.3099967661951,10.2414594521436,-6.50694623445706));
#18216=CARTESIAN_POINT('Ctrl Pts',(13.1203496652059,10.1290900041791,-6.36108719500251));
#18217=CARTESIAN_POINT('Ctrl Pts',(12.9320806449423,10.0171093135792,-6.21604099337274));
#18218=CARTESIAN_POINT('Ctrl Pts',(12.7398364624418,9.9027642328534,-6.06793224761062));
#18219=CARTESIAN_POINT('Ctrl Pts',(12.5465418490568,9.78738841037906,-5.91877633502142));
#18220=CARTESIAN_POINT('Ctrl Pts',(12.3528703671111,9.67121625884532,-5.76903486398257));
#18221=CARTESIAN_POINT('Ctrl Pts',(12.1588882142736,9.55485775408309,-5.61905319074209));
#18222=CARTESIAN_POINT('Ctrl Pts',(11.9645279828264,9.43770055909591,-5.46848389786619));
#18223=CARTESIAN_POINT('Ctrl Pts',(11.7704664817053,9.32001254164005,-5.31783217681151));
#18224=CARTESIAN_POINT('Ctrl Pts',(11.5758141145056,9.20196619521644,-5.16672176100727));
#18225=CARTESIAN_POINT('Ctrl Pts',(11.3814622995116,9.08338602074528,-5.01552828296685));
#18226=CARTESIAN_POINT('Ctrl Pts',(11.1880940466152,8.96457159711152,-4.86480554216724));
#18227=CARTESIAN_POINT('Ctrl Pts',(10.9918680747371,8.84400125838504,-4.71185532487703));
#18228=CARTESIAN_POINT('Ctrl Pts',(10.7966549511866,8.72318989747891,-4.55938973719067));
#18229=CARTESIAN_POINT('Ctrl Pts',(10.6031684174481,8.60247741697815,-4.40803483976878));
#18230=CARTESIAN_POINT('Ctrl Pts',(10.4170538516967,8.4863641637451,-4.26244666645391));
#18231=CARTESIAN_POINT('Ctrl Pts',(10.232536813699,8.37034275782415,-4.11788655117324));
#18232=CARTESIAN_POINT('Ctrl Pts',(10.0502525316942,8.25473589028142,-3.97495252086484));
#18233=CARTESIAN_POINT('Ctrl Pts',(15.8,11.6949834819563,-8.4075644298998));
#18234=CARTESIAN_POINT('Ctrl Pts',(15.8,11.7024865012679,-8.41193022268479));
#18235=CARTESIAN_POINT('Ctrl Pts',(15.8,11.709964652185,-8.41633052040236));
#18236=CARTESIAN_POINT('Ctrl Pts',(15.8,11.7174179347465,-8.4207653230234));
#18237=CARTESIAN_POINT('Ctrl Pts',(15.8,11.7248463432757,-8.4252346384098));
#18238=CARTESIAN_POINT('Ctrl Pts',(15.8,11.7322498653003,-8.42973848206085));
#18239=CARTESIAN_POINT('Ctrl Pts',(10.0502525316942,6.62239247796684,-6.33125817110613));
#18240=CARTESIAN_POINT('Ctrl Pts',(11.9668350211294,7.25643163809036,-8.09084464143287));
#18241=CARTESIAN_POINT('Ctrl Pts',(13.8834175105647,7.89047079821388,-9.85043111175961));
#18242=CARTESIAN_POINT('Ctrl Pts',(15.8,8.5245099583374,-11.6100175820864));
#18243=CARTESIAN_POINT('Ctrl Pts',(10.0502525316942,6.74536016772826,-6.42803507865412));
#18244=CARTESIAN_POINT('Ctrl Pts',(11.9668350211294,7.39344597705573,-8.21671225999592));
#18245=CARTESIAN_POINT('Ctrl Pts',(13.8834175105647,8.04138429933134,-10.0057987839539));
#18246=CARTESIAN_POINT('Ctrl Pts',(15.8,8.68947010865881,-11.7944759652957));
#18247=CARTESIAN_POINT('Ctrl Pts',(10.0502525316942,6.95639005916885,-6.65988565896846));
#18248=CARTESIAN_POINT('Ctrl Pts',(11.9668350211295,7.62236086025717,-8.51136454012836));
#18249=CARTESIAN_POINT('Ctrl Pts',(13.8834175105647,8.28779124445876,-10.3629488876586));
#18250=CARTESIAN_POINT('Ctrl Pts',(15.8,8.95376204554707,-12.2144277688185));
#18251=CARTESIAN_POINT('Ctrl Pts',(10.0502525316941,7.17140112925238,-7.20716777578593));
#18252=CARTESIAN_POINT('Ctrl Pts',(11.9668350211294,7.82602495118042,-9.17886046565846));
#18253=CARTESIAN_POINT('Ctrl Pts',(13.8834175105647,8.48103967091343,-11.1506718004078));
#18254=CARTESIAN_POINT('Ctrl Pts',(15.8,9.13566349284146,-13.1223644902804));
#18255=CARTESIAN_POINT('Ctrl Pts',(10.0502525316942,7.25121893082227,-7.64992225296746));
#18256=CARTESIAN_POINT('Ctrl Pts',(11.9668350211294,7.88043377854935,-9.70870355968973));
#18257=CARTESIAN_POINT('Ctrl Pts',(13.8834175105647,8.50859598070372,-11.7676943247925));
#18258=CARTESIAN_POINT('Ctrl Pts',(15.8,9.13781082843079,-13.8264756315147));
#18259=CARTESIAN_POINT('Ctrl Pts',(10.0502525316942,7.27527035012649,-7.92891439885425));
#18260=CARTESIAN_POINT('Ctrl Pts',(11.9668350211294,7.88323296009842,-10.0398646795257));
#18261=CARTESIAN_POINT('Ctrl Pts',(13.8834175105647,8.49119557007034,-12.1508149601973));
#18262=CARTESIAN_POINT('Ctrl Pts',(15.8,9.09915818004226,-14.2617652408688));
#18263=CARTESIAN_POINT('',(10.0502525316942,7.27527035012649,-7.92891439885425));
#18264=CARTESIAN_POINT('',(15.8,8.5245099583374,-11.6100175820864));
#18265=CARTESIAN_POINT('Ctrl Pts',(15.8,8.5245099583374,-11.6100175820864));
#18266=CARTESIAN_POINT('Ctrl Pts',(15.5486176754283,8.44542381127122,-11.3837844012201));
#18267=CARTESIAN_POINT('Ctrl Pts',(15.2955013981408,8.36553547761206,-11.1556103968136));
#18268=CARTESIAN_POINT('Ctrl Pts',(15.0417459576106,8.28507970174558,-10.9263572847368));
#18269=CARTESIAN_POINT('Ctrl Pts',(14.7869004713578,8.20427831565627,-10.696119380477));
#18270=CARTESIAN_POINT('Ctrl Pts',(14.531410318819,8.12290482377608,-10.4647929695858));
#18271=CARTESIAN_POINT('Ctrl Pts',(14.2763844586717,8.0412226669247,-10.2332972079364));
#18272=CARTESIAN_POINT('Ctrl Pts',(14.0169022052172,7.95811317318716,-9.99775622451133));
#18273=CARTESIAN_POINT('Ctrl Pts',(13.7579006122767,7.87468439208872,-9.76203981942054));
#18274=CARTESIAN_POINT('Ctrl Pts',(13.5005477950714,7.79123671760748,-9.52716576584172));
#18275=CARTESIAN_POINT('Ctrl Pts',(13.30999677658,7.72944979203263,-9.35325863471847));
#18276=CARTESIAN_POINT('Ctrl Pts',(13.1203496703607,7.66765301700974,-9.1798143702817));
#18277=CARTESIAN_POINT('Ctrl Pts',(12.9320806449423,7.605974791296,-9.00726329348628));
#18278=CARTESIAN_POINT('Ctrl Pts',(12.7398364200678,7.54299426293975,-8.83106889328651));
#18279=CARTESIAN_POINT('Ctrl Pts',(12.5465417638457,7.47935703277434,-8.65356006118378));
#18280=CARTESIAN_POINT('Ctrl Pts',(12.3528702390454,7.41514339569062,-8.47524825078843));
#18281=CARTESIAN_POINT('Ctrl Pts',(12.1588880967136,7.35082677040844,-8.29665045733793));
#18282=CARTESIAN_POINT('Ctrl Pts',(11.9645278759626,7.28593212986481,-8.11724699610014));
#18283=CARTESIAN_POINT('Ctrl Pts',(11.7704663856167,7.22055811872365,-7.9376011083099));
#18284=CARTESIAN_POINT('Ctrl Pts',(11.5758138300784,7.15498499387682,-7.75740806182766));
#18285=CARTESIAN_POINT('Ctrl Pts',(11.3814618274401,7.08892983490276,-7.57697105649293));
#18286=CARTESIAN_POINT('Ctrl Pts',(11.1880933895773,7.02250642528014,-7.39690936354705));
#18287=CARTESIAN_POINT('Ctrl Pts',(10.99186689856,6.95510125442749,-7.21418629579141));
#18288=CARTESIAN_POINT('Ctrl Pts',(10.7966532620494,6.88731709712089,-7.03184966122165));
#18289=CARTESIAN_POINT('Ctrl Pts',(10.6031662272196,6.81928375787422,-6.85059991984744));
#18290=CARTESIAN_POINT('Ctrl Pts',(10.4170524040777,6.75384296552633,-6.67625706354029));
#18291=CARTESIAN_POINT('Ctrl Pts',(10.2325360986479,6.68817184019669,-6.50292032538242));
#18292=CARTESIAN_POINT('Ctrl Pts',(10.0502525316942,6.62239247796684,-6.33125817110613));
#18293=CARTESIAN_POINT('Ctrl Pts',(15.8,8.5245099583374,-11.6100175820864));
#18294=CARTESIAN_POINT('Ctrl Pts',(15.8,8.53029664958107,-11.6164882582397));
#18295=CARTESIAN_POINT('Ctrl Pts',(15.8,8.53604902696561,-11.6229840657775));
#18296=CARTESIAN_POINT('Ctrl Pts',(15.8,8.54176709053684,-11.6295050046841));
#18297=CARTESIAN_POINT('Ctrl Pts',(15.8,8.54745083246671,-11.6360510806824));
#18298=CARTESIAN_POINT('Ctrl Pts',(15.8,8.55310023610356,-11.642622304659));
#18299=CARTESIAN_POINT('Ctrl Pts',(10.0502525316942,4.34180314898733,-8.06781615908999));
#18300=CARTESIAN_POINT('Ctrl Pts',(11.9668350211294,4.40106810140592,-9.93721121325641));
#18301=CARTESIAN_POINT('Ctrl Pts',(13.8834175105647,4.46033305382451,-11.8066062674228));
#18302=CARTESIAN_POINT('Ctrl Pts',(15.8,4.51959800624309,-13.6760013215893));
#18303=CARTESIAN_POINT('Ctrl Pts',(10.0502525316942,4.4288466625333,-8.19785557353568));
#18304=CARTESIAN_POINT('Ctrl Pts',(11.9668350211294,4.49248124812732,-10.0992581912947));
#18305=CARTESIAN_POINT('Ctrl Pts',(13.8834175105647,4.55584907137465,-12.0010045410108));
#18306=CARTESIAN_POINT('Ctrl Pts',(15.8,4.61948365696867,-13.9024071587698));
#18307=CARTESIAN_POINT('Ctrl Pts',(10.0502525316942,4.55790932427761,-8.48356457498289));
#18308=CARTESIAN_POINT('Ctrl Pts',(11.9668350211294,4.61914675531023,-10.4502219249867));
#18309=CARTESIAN_POINT('Ctrl Pts',(13.8834175105647,4.67984453466857,-12.416810143598));
#18310=CARTESIAN_POINT('Ctrl Pts',(15.8,4.74108196570119,-14.3834674936017));
#18311=CARTESIAN_POINT('Ctrl Pts',(10.0502525316941,4.59327853800038,-9.07050287838802));
#18312=CARTESIAN_POINT('Ctrl Pts',(11.9668350211294,4.60657624071161,-11.1479839451212));
#18313=CARTESIAN_POINT('Ctrl Pts',(13.8834175105647,4.62021662092399,-13.2256962639304));
#18314=CARTESIAN_POINT('Ctrl Pts',(15.8,4.63351432363523,-15.3031773306636));
#18315=CARTESIAN_POINT('Ctrl Pts',(10.0502525316942,4.5323630334273,-9.51625828739342));
#18316=CARTESIAN_POINT('Ctrl Pts',(11.9668350211294,4.49458350302914,-11.668713745839));
#18317=CARTESIAN_POINT('Ctrl Pts',(13.8834175105647,4.45573812100051,-13.8210431256713));
#18318=CARTESIAN_POINT('Ctrl Pts',(15.8,4.41795859060236,-15.9734985841168));
#18319=CARTESIAN_POINT('Ctrl Pts',(10.0502525316942,4.46902397810654,-9.78902788303806));
#18320=CARTESIAN_POINT('Ctrl Pts',(11.9668350211294,4.39491126897609,-11.9845316814717));
#18321=CARTESIAN_POINT('Ctrl Pts',(13.8834175105647,4.32079855984563,-14.1800354799052));
#18322=CARTESIAN_POINT('Ctrl Pts',(15.8,4.24668585071518,-16.3755392783388));
#18323=CARTESIAN_POINT('',(10.0502525316942,4.46902397810654,-9.78902788303806));
#18324=CARTESIAN_POINT('',(15.8,4.51959800624309,-13.6760013215893));
#18325=CARTESIAN_POINT('Ctrl Pts',(15.8,4.51959800624309,-13.6760013215893));
#18326=CARTESIAN_POINT('Ctrl Pts',(15.5486181428678,4.51429251817175,-13.4364022627908));
#18327=CARTESIAN_POINT('Ctrl Pts',(15.2955023394683,4.50882385781799,-13.1947094870259));
#18328=CARTESIAN_POINT('Ctrl Pts',(15.0417473731674,4.50314899406868,-12.9518150706376));
#18329=CARTESIAN_POINT('Ctrl Pts',(14.7869020465192,4.49744974598318,-12.7078769606258));
#18330=CARTESIAN_POINT('Ctrl Pts',(14.5314120523271,4.49154276300949,-12.4627268269524));
#18331=CARTESIAN_POINT('Ctrl Pts',(14.2763863472162,4.48539455472627,-12.2173202460906));
#18332=CARTESIAN_POINT('Ctrl Pts',(14.0169034957089,4.4791388927086,-11.9676246346112));
#18333=CARTESIAN_POINT('Ctrl Pts',(13.7579013040888,4.47263377735531,-11.7176635180578));
#18334=CARTESIAN_POINT('Ctrl Pts',(13.5005478956223,4.46585038850025,-11.4684976917997));
#18335=CARTESIAN_POINT('Ctrl Pts',(13.3099968432959,4.46082779372533,-11.2840089349569));
#18336=CARTESIAN_POINT('Ctrl Pts',(13.1203497034762,4.45565279642652,-11.0999573476245));
#18337=CARTESIAN_POINT('Ctrl Pts',(12.9320806449423,4.45031453415308,-10.9167918673754));
#18338=CARTESIAN_POINT('Ctrl Pts',(12.7398361468871,4.44486355054889,-10.729758713411));
#18339=CARTESIAN_POINT('Ctrl Pts',(12.5465412144991,4.43919418585341,-10.5412725252545));
#18340=CARTESIAN_POINT('Ctrl Pts',(12.3528694134188,4.4332247563449,-10.3518445394593));
#18341=CARTESIAN_POINT('Ctrl Pts',(12.1588873388164,4.42724576346212,-10.1621130789817));
#18342=CARTESIAN_POINT('Ctrl Pts',(11.9645271870233,4.42096600829023,-9.97143676938844));
#18343=CARTESIAN_POINT('Ctrl Pts',(11.7704657661435,4.41430525673782,-9.78038176737572));
#18344=CARTESIAN_POINT('Ctrl Pts',(11.5758119966791,4.4076241740617,-9.58874359350173));
#18345=CARTESIAN_POINT('Ctrl Pts',(11.3814587845899,4.40056003028008,-9.39672444178994));
#18346=CARTESIAN_POINT('Ctrl Pts',(11.1880891545369,4.39302967416939,-9.20494844642816));
#18347=CARTESIAN_POINT('Ctrl Pts',(10.9918593168755,4.3853879335469,-9.01033581554672));
#18348=CARTESIAN_POINT('Ctrl Pts',(10.796642373555,4.37726632301398,-8.81597360566157));
#18349=CARTESIAN_POINT('Ctrl Pts',(10.6031521084281,4.36857183761346,-8.62256814054944));
#18350=CARTESIAN_POINT('Ctrl Pts',(10.4170430723424,4.36020902775276,-8.43654066954402));
#18351=CARTESIAN_POINT('Ctrl Pts',(10.2325314892389,4.35131627654661,-8.25139886794601));
#18352=CARTESIAN_POINT('Ctrl Pts',(10.0502525316942,4.34180314898733,-8.06781615908999));
#18353=CARTESIAN_POINT('Ctrl Pts',(15.8,4.51959800624309,-13.6760013215893));
#18354=CARTESIAN_POINT('Ctrl Pts',(15.8,4.52310192776169,-13.6839434862452));
#18355=CARTESIAN_POINT('Ctrl Pts',(15.8,4.52656544883607,-13.6918989487026));
#18356=CARTESIAN_POINT('Ctrl Pts',(15.8,4.52998856951466,-13.6998677089605));
#18357=CARTESIAN_POINT('Ctrl Pts',(15.8,4.53337128058405,-13.7078497700428));
#18358=CARTESIAN_POINT('Ctrl Pts',(15.8,4.53671356284346,-13.7158451371576));
#18359=CARTESIAN_POINT('Ctrl Pts',(10.0502525316942,1.6362078766636,-9.01464008964162));
#18360=CARTESIAN_POINT('Ctrl Pts',(11.9668350211294,1.11489735491132,-10.8108543149047));
#18361=CARTESIAN_POINT('Ctrl Pts',(13.8834175105647,0.593586833159036,-12.6070685401678));
#18362=CARTESIAN_POINT('Ctrl Pts',(15.8,0.0722763114067552,-14.4032827654308));
#18363=CARTESIAN_POINT('Ctrl Pts',(10.0502525316942,1.67880678842043,-9.16521284706123));
#18364=CARTESIAN_POINT('Ctrl Pts',(11.9668350211294,1.15176115367482,-10.9932183651601));
#18365=CARTESIAN_POINT('Ctrl Pts',(13.8834175105647,0.624355593844835,-12.8214683576781));
#18366=CARTESIAN_POINT('Ctrl Pts',(15.8,0.0973099590992221,-14.6494738757771));
#18367=CARTESIAN_POINT('Ctrl Pts',(10.0502525316942,1.71327315824379,-9.47681709721301));
#18368=CARTESIAN_POINT('Ctrl Pts',(11.9668350211294,1.16378287280497,-11.3661427921348));
#18369=CARTESIAN_POINT('Ctrl Pts',(13.8834175105647,0.613808798404413,-13.2552357701884));
#18370=CARTESIAN_POINT('Ctrl Pts',(15.8,0.064318512965595,-15.1445614651102));
#18371=CARTESIAN_POINT('Ctrl Pts',(10.0502525316941,1.56553830329485,-10.0459586957056));
#18372=CARTESIAN_POINT('Ctrl Pts',(11.9668350211294,0.936208214997359,-12.025869817826));
#18373=CARTESIAN_POINT('Ctrl Pts',(13.8834175105647,0.307141231238404,-14.0061068566225));
#18374=CARTESIAN_POINT('Ctrl Pts',(15.8,-0.322188857059085,-15.9860179787428));
#18375=CARTESIAN_POINT('Ctrl Pts',(10.0502525316942,1.36984786349029,-10.4510766569791));
#18376=CARTESIAN_POINT('Ctrl Pts',(11.9668350211294,0.668772078627757,-12.4865089298363));
#18377=CARTESIAN_POINT('Ctrl Pts',(13.8834175105647,-0.0332784309391876,
-14.5214919285394));
#18378=CARTESIAN_POINT('Ctrl Pts',(15.8,-0.734354215801725,-16.5569242013966));
#18379=CARTESIAN_POINT('Ctrl Pts',(10.0502525316942,1.22531840158854,-10.6909231138624));
#18380=CARTESIAN_POINT('Ctrl Pts',(11.9668350211294,0.476385041699009,-12.7560692212929));
#18381=CARTESIAN_POINT('Ctrl Pts',(13.8834175105647,-0.272548318190526,
-14.8212153287235));
#18382=CARTESIAN_POINT('Ctrl Pts',(15.8,-1.02148167808006,-16.886361436154));
#18383=CARTESIAN_POINT('',(10.0502525316942,1.22531840158854,-10.6909231138624));
#18384=CARTESIAN_POINT('',(15.8,0.0722763114067552,-14.4032827654308));
#18385=CARTESIAN_POINT('Ctrl Pts',(15.8,0.0722763114067553,-14.4032827654308));
#18386=CARTESIAN_POINT('Ctrl Pts',(15.5486186601036,0.141270531448607,-14.1737715055214));
#18387=CARTESIAN_POINT('Ctrl Pts',(15.2955033810753,0.210756563075219,-13.9422185866342));
#18388=CARTESIAN_POINT('Ctrl Pts',(15.0417489395233,0.280417814421832,-13.7094591215782));
#18389=CARTESIAN_POINT('Ctrl Pts',(14.7869037890756,0.35037848967631,-13.4756991900179));
#18390=CARTESIAN_POINT('Ctrl Pts',(14.5314139696902,0.42051613703443,-13.2407223608425));
#18391=CARTESIAN_POINT('Ctrl Pts',(14.2763884357263,0.490503613096802,-13.005427090821));
#18392=CARTESIAN_POINT('Ctrl Pts',(14.0169049225921,0.561714506695558,-12.7660187369198));
#18393=CARTESIAN_POINT('Ctrl Pts',(13.7579020686525,0.632770201645049,-12.5262807827892));
#18394=CARTESIAN_POINT('Ctrl Pts',(13.5005480060748,0.703315478824952,-12.2872132071322));
#18395=CARTESIAN_POINT('Ctrl Pts',(13.3099969165817,0.755548885558801,-12.1102018689483));
#18396=CARTESIAN_POINT('Ctrl Pts',(13.1203497398528,0.807502254261702,-11.9335592090234));
#18397=CARTESIAN_POINT('Ctrl Pts',(12.9320806449423,0.859026524117212,-11.7577088361878));
#18398=CARTESIAN_POINT('Ctrl Pts',(12.7398358447889,0.911638839304298,-11.578145006029));
#18399=CARTESIAN_POINT('Ctrl Pts',(12.5465406070012,0.964492472594393,-11.3971317706528));
#18400=CARTESIAN_POINT('Ctrl Pts',(12.3528685003953,1.0173517555332,-11.215130105891));
#18401=CARTESIAN_POINT('Ctrl Pts',(12.1588865006919,1.07029561816294,-11.0328372218068));
#18402=CARTESIAN_POINT('Ctrl Pts',(11.9645264251562,1.12324541000608,-10.8495527946017));
#18403=CARTESIAN_POINT('Ctrl Pts',(11.7704650810958,1.17594987240342,-10.66579047727));
#18404=CARTESIAN_POINT('Ctrl Pts',(11.575809969755,1.22881559404307,-10.4814659044725));
#18405=CARTESIAN_POINT('Ctrl Pts',(11.3814554207367,1.28143472519663,-10.2966606229241));
#18406=CARTESIAN_POINT('Ctrl Pts',(11.188084472835,1.33353531202393,-10.1119425360162));
#18407=CARTESIAN_POINT('Ctrl Pts',(10.9918509346328,1.38640717621279,-9.92448995248599));
#18408=CARTESIAN_POINT('Ctrl Pts',(10.7966303348178,1.43874524883781,-9.73712725458209));
#18409=CARTESIAN_POINT('Ctrl Pts',(10.6031364978011,1.49024279648084,-9.5504974919454));
#18410=CARTESIAN_POINT('Ctrl Pts',(10.4170327545854,1.5397735026292,-9.37099566409577));
#18411=CARTESIAN_POINT('Ctrl Pts',(10.2325263927829,1.58852655489966,-9.19217237538429));
#18412=CARTESIAN_POINT('Ctrl Pts',(10.0502525316942,1.6362078766636,-9.01464008964162));
#18413=CARTESIAN_POINT('Ctrl Pts',(15.8,0.0722763114067552,-14.4032827654308));
#18414=CARTESIAN_POINT('Ctrl Pts',(15.8,0.07315447494878,-14.4119189841766));
#18415=CARTESIAN_POINT('Ctrl Pts',(15.8,0.073990106138469,-14.4205553654592));
#18416=CARTESIAN_POINT('Ctrl Pts',(15.8,0.0747832050221156,-14.4291919092927));
#18417=CARTESIAN_POINT('Ctrl Pts',(15.8,0.0755337619028261,-14.437828615706));
#18418=CARTESIAN_POINT('Ctrl Pts',(15.8,0.0762417569101966,-14.4464654837189));
#18419=CARTESIAN_POINT('Ctrl Pts',(10.0502525316942,-1.22955082275859,-9.07904823952839));
#18420=CARTESIAN_POINT('Ctrl Pts',(11.9668350211294,-2.28040731262864,-10.626255672559));
#18421=CARTESIAN_POINT('Ctrl Pts',(13.8834175105647,-3.33126380249869,-12.1734631055895));
#18422=CARTESIAN_POINT('Ctrl Pts',(15.8,-4.38212029236875,-13.7206705386201));
#18423=CARTESIAN_POINT('Ctrl Pts',(10.0502525316942,-1.23556639107773,-9.23541522932356));
#18424=CARTESIAN_POINT('Ctrl Pts',(11.9668350211294,-2.3017013472912,-10.8110857311875));
#18425=CARTESIAN_POINT('Ctrl Pts',(13.8834175105647,-3.36825415935173,-12.3868775190731));
#18426=CARTESIAN_POINT('Ctrl Pts',(15.8,-4.43438911556521,-13.962548020937));
#18427=CARTESIAN_POINT('Ctrl Pts',(10.0502525316942,-1.29909254545997,-9.54242006948553));
#18428=CARTESIAN_POINT('Ctrl Pts',(11.9668350211294,-2.40552260970754,-11.1694737466002));
#18429=CARTESIAN_POINT('Ctrl Pts',(13.8834175105647,-3.51235208206866,-12.7961532691502));
#18430=CARTESIAN_POINT('Ctrl Pts',(15.8,-4.61878214631622,-14.4232069462649));
#18431=CARTESIAN_POINT('Ctrl Pts',(10.0502525316941,-1.6154723149753,-10.0380523375239));
#18432=CARTESIAN_POINT('Ctrl Pts',(11.9668350211294,-2.82582698043839,-11.7265860195463));
#18433=CARTESIAN_POINT('Ctrl Pts',(13.8834175105647,-4.03604403376329,-13.4155069687333));
#18434=CARTESIAN_POINT('Ctrl Pts',(15.8,-5.24639869922639,-15.1040406507558));
#18435=CARTESIAN_POINT('Ctrl Pts',(10.0502525316942,-1.92675755961641,-10.3628708264469));
#18436=CARTESIAN_POINT('Ctrl Pts',(11.9668350211294,-3.22250341643877,-12.0820376211579));
#18437=CARTESIAN_POINT('Ctrl Pts',(13.8834175105647,-4.51903745819409,-13.8004759242586));
#18438=CARTESIAN_POINT('Ctrl Pts',(15.8,-5.81478331501644,-15.5196427189696));
#18439=CARTESIAN_POINT('Ctrl Pts',(10.0502525316942,-2.13832987737225,-10.5463163022605));
#18440=CARTESIAN_POINT('Ctrl Pts',(11.9668350211294,-3.48877307262933,-12.2789538289737));
#18441=CARTESIAN_POINT('Ctrl Pts',(13.8834175105647,-4.8392162678864,-14.0115913556869));
#18442=CARTESIAN_POINT('Ctrl Pts',(15.8,-6.18965946314348,-15.7442288824001));
#18443=CARTESIAN_POINT('',(10.0502525316942,-2.13832987737225,-10.5463163022605));
#18444=CARTESIAN_POINT('',(15.8,-4.38212029236875,-13.7206705386201));
#18445=CARTESIAN_POINT('Ctrl Pts',(15.8,-4.38212029236875,-13.7206705386201));
#18446=CARTESIAN_POINT('Ctrl Pts',(15.5486179127196,-4.24557960414972,-13.5237121602497));
#18447=CARTESIAN_POINT('Ctrl Pts',(15.295501875997,-4.10794026962981,-13.3249640154802));
#18448=CARTESIAN_POINT('Ctrl Pts',(15.0417466762049,-3.96976145165723,-13.1251225182518));
#18449=CARTESIAN_POINT('Ctrl Pts',(14.7869012710178,-3.83098897770061,-12.9244224444165));
#18450=CARTESIAN_POINT('Ctrl Pts',(14.5314111989065,-3.69167215691846,-12.7226197192354));
#18451=CARTESIAN_POINT('Ctrl Pts',(14.2763854175058,-3.55239975641227,-12.5204677360921));
#18452=CARTESIAN_POINT('Ctrl Pts',(14.0169028604397,-3.41069346141101,-12.3147829884013));
#18453=CARTESIAN_POINT('Ctrl Pts',(13.7579009635692,-3.26903291905704,-12.1087368195414));
#18454=CARTESIAN_POINT('Ctrl Pts',(13.5005478461999,-3.12806496166868,-11.9031704882092));
#18455=CARTESIAN_POINT('Ctrl Pts',(13.309996810504,-3.02368856803927,-11.750963754753));
#18456=CARTESIAN_POINT('Ctrl Pts',(13.1203496871994,-2.91969243162214,-11.5990211190191));
#18457=CARTESIAN_POINT('Ctrl Pts',(12.9320806449423,-2.81634921885376,-11.4476993942222));
#18458=CARTESIAN_POINT('Ctrl Pts',(12.7398362813702,-2.71082390290183,-11.2931824947393));
#18459=CARTESIAN_POINT('Ctrl Pts',(12.5465414849348,-2.6046211888686,-11.1373617066502));
#18460=CARTESIAN_POINT('Ctrl Pts',(12.3528698198632,-2.49810765643983,-10.9806026156652));
#18461=CARTESIAN_POINT('Ctrl Pts',(12.1588877119187,-2.39142338986155,-10.8235922502227));
#18462=CARTESIAN_POINT('Ctrl Pts',(11.9645275261786,-2.28442707498171,-10.6656407015677));
#18463=CARTESIAN_POINT('Ctrl Pts',(11.7704660711016,-2.17751640137217,-10.5071588397361));
#18464=CARTESIAN_POINT('Ctrl Pts',(11.5758128991787,-2.07027974418926,-10.3481937475414));
#18465=CARTESIAN_POINT('Ctrl Pts',(11.3814602824281,-1.96312905478001,-10.1886952830847));
#18466=CARTESIAN_POINT('Ctrl Pts',(11.1880912392172,-1.85649845736375,-10.029119502121));
#18467=CARTESIAN_POINT('Ctrl Pts',(10.9918630490257,-1.74829122417593,-9.86718424000794));
#18468=CARTESIAN_POINT('Ctrl Pts',(10.7966477335658,-1.64061939633818,-9.70516951171922));
#18469=CARTESIAN_POINT('Ctrl Pts',(10.603159058634,-1.53397337210466,-9.54359206502157));
#18470=CARTESIAN_POINT('Ctrl Pts',(10.4170476660417,-1.43139351779785,-9.38817519823602));
#18471=CARTESIAN_POINT('Ctrl Pts',(10.2325337582961,-1.32976299718735,-9.23316336539122));
#18472=CARTESIAN_POINT('Ctrl Pts',(10.0502525316942,-1.22955082275859,-9.07904823952839));
#18473=CARTESIAN_POINT('Ctrl Pts',(15.8,-4.38212029236875,-13.7206705386201));
#18474=CARTESIAN_POINT('Ctrl Pts',(15.8,-4.38395384756931,-13.7291554381927));
#18475=CARTESIAN_POINT('Ctrl Pts',(15.8,-4.38582790366735,-13.7376273491274));
#18476=CARTESIAN_POINT('Ctrl Pts',(15.8,-4.38774246062322,-13.7460862714518));
#18477=CARTESIAN_POINT('Ctrl Pts',(15.8,-4.38969752766812,-13.7545322021969));
#18478=CARTESIAN_POINT('Ctrl Pts',(15.8,-4.391693123397,-13.7629651342901));
#18479=CARTESIAN_POINT('Ctrl Pts',(10.0502525316942,-3.97495252086484,-8.25473589028142));
#18480=CARTESIAN_POINT('Ctrl Pts',(11.9668350211294,-5.45248982387649,-9.40148508750639));
#18481=CARTESIAN_POINT('Ctrl Pts',(13.8834175105647,-6.93002712688815,-10.5482342847314));
#18482=CARTESIAN_POINT('Ctrl Pts',(15.8,-8.40756442989979,-11.6949834819563));
#18483=CARTESIAN_POINT('Ctrl Pts',(10.0502525316942,-4.02899372351993,-8.40159082201815));
#18484=CARTESIAN_POINT('Ctrl Pts',(11.9668350211294,-5.52985728348807,-9.57068870058276));
#18485=CARTESIAN_POINT('Ctrl Pts',(13.8834175105647,-7.03115572742428,-10.7397728044506));
#18486=CARTESIAN_POINT('Ctrl Pts',(15.8,-8.53201928739242,-11.9088706830152));
#18487=CARTESIAN_POINT('Ctrl Pts',(10.0502525316942,-4.18428628311193,-8.6739375870516));
#18488=CARTESIAN_POINT('Ctrl Pts',(11.9668350211294,-5.73935104252813,-9.87945189609367));
#18489=CARTESIAN_POINT('Ctrl Pts',(13.8834175105647,-7.29468404041881,-11.0844841840221));
#18490=CARTESIAN_POINT('Ctrl Pts',(15.8,-8.84974879983501,-12.2899984930642));
#18491=CARTESIAN_POINT('Ctrl Pts',(10.0502525316941,-4.63834053369691,-9.04754461221301));
#18492=CARTESIAN_POINT('Ctrl Pts',(11.9668350211294,-6.31124182863326,-10.2794154126352));
#18493=CARTESIAN_POINT('Ctrl Pts',(13.8834175105647,-7.98413616433457,-11.5116939035746));
#18494=CARTESIAN_POINT('Ctrl Pts',(15.8,-9.65703745927091,-12.7435647039968));
#18495=CARTESIAN_POINT('Ctrl Pts',(10.0502525316942,-5.0347585282786,-9.26027499705532));
#18496=CARTESIAN_POINT('Ctrl Pts',(11.9668350211294,-6.79833782460276,-10.4948922896145));
#18497=CARTESIAN_POINT('Ctrl Pts',(13.8834175105647,-8.56244161305558,-11.7285731829415));
#18498=CARTESIAN_POINT('Ctrl Pts',(15.8,-10.3260209093797,-12.9631904755006));
#18499=CARTESIAN_POINT('Ctrl Pts',(10.0502525316942,-5.29266352931554,-9.36936257048691));
#18500=CARTESIAN_POINT('Ctrl Pts',(11.9668350211294,-7.11242577089738,-10.5998888833726));
#18501=CARTESIAN_POINT('Ctrl Pts',(13.8834175105647,-8.93218801247923,-11.8304151962582));
#18502=CARTESIAN_POINT('Ctrl Pts',(15.8,-10.7519502540611,-13.0609415091439));
#18503=CARTESIAN_POINT('',(10.0502525316942,-5.29266352931554,-9.36936257048691));
#18504=CARTESIAN_POINT('',(15.8,-8.40756442989979,-11.6949834819563));
#18505=CARTESIAN_POINT('Ctrl Pts',(15.8,-8.40756442989979,-11.6949834819563));
#18506=CARTESIAN_POINT('Ctrl Pts',(15.5486176029454,-8.21684279750569,-11.5498581470161));
#18507=CARTESIAN_POINT('Ctrl Pts',(15.295501252175,-8.02452322133501,-11.4033701387249));
#18508=CARTESIAN_POINT('Ctrl Pts',(15.0417457381091,-7.83135270226614,-11.2560089976682));
#18509=CARTESIAN_POINT('Ctrl Pts',(14.786900227078,-7.63735242672743,-11.1080148725475));
#18510=CARTESIAN_POINT('Ctrl Pts',(14.5314100499558,-7.44249371079127,-10.9591402752368));
#18511=CARTESIAN_POINT('Ctrl Pts',(14.2763841657387,-7.24756931575029,-10.8099197880108));
#18512=CARTESIAN_POINT('Ctrl Pts',(14.0169020050304,-7.04923884684419,-10.6580918487951));
#18513=CARTESIAN_POINT('Ctrl Pts',(13.7579005049334,-6.85084020761701,-10.5059060414985));
#18514=CARTESIAN_POINT('Ctrl Pts',(13.5005477794214,-6.6532485297061,-10.3539625665131));
#18515=CARTESIAN_POINT('Ctrl Pts',(13.3099967661962,-6.50694623445787,-10.2414594521442));
#18516=CARTESIAN_POINT('Ctrl Pts',(13.1203496652064,-6.36108719500292,-10.1290900041794));
#18517=CARTESIAN_POINT('Ctrl Pts',(12.9320806449423,-6.21604099337274,-10.0171093135792));
#18518=CARTESIAN_POINT('Ctrl Pts',(12.7398364624423,-6.06793224761101,-9.90276423285371));
#18519=CARTESIAN_POINT('Ctrl Pts',(12.5465418490578,-5.91877633502221,-9.78738841037967));
#18520=CARTESIAN_POINT('Ctrl Pts',(12.3528703671126,-5.76903486398375,-9.67121625884623));
#18521=CARTESIAN_POINT('Ctrl Pts',(12.158888214275,-5.61905319074317,-9.55485775408393));
#18522=CARTESIAN_POINT('Ctrl Pts',(11.9645279828276,-5.46848389786717,-9.43770055909668));
#18523=CARTESIAN_POINT('Ctrl Pts',(11.7704664817065,-5.3178321768124,-9.32001254164074));
#18524=CARTESIAN_POINT('Ctrl Pts',(11.5758141145072,-5.16672176100845,-9.20196619521737));
#18525=CARTESIAN_POINT('Ctrl Pts',(11.3814622995135,-5.01552828296833,-9.08338602074645));
#18526=CARTESIAN_POINT('Ctrl Pts',(11.1880940466175,-4.86480554216901,-8.96457159711292));
#18527=CARTESIAN_POINT('Ctrl Pts',(10.9918680747393,-4.71185532487872,-8.84400125838637));
#18528=CARTESIAN_POINT('Ctrl Pts',(10.7966549511886,-4.55938973719227,-8.72318989748018));
#18529=CARTESIAN_POINT('Ctrl Pts',(10.60316841745,-4.40803483977029,-8.60247741697936));
#18530=CARTESIAN_POINT('Ctrl Pts',(10.417053851698,-4.26244666645491,-8.4863641637459));
#18531=CARTESIAN_POINT('Ctrl Pts',(10.2325368136996,-4.11788655117373,-8.37034275782455));
#18532=CARTESIAN_POINT('Ctrl Pts',(10.0502525316942,-3.97495252086484,-8.25473589028142));
#18533=CARTESIAN_POINT('Ctrl Pts',(15.8,-8.40756442989979,-11.6949834819563));
#18534=CARTESIAN_POINT('Ctrl Pts',(15.8,-8.41193022268479,-11.7024865012679));
#18535=CARTESIAN_POINT('Ctrl Pts',(15.8,-8.41633052040236,-11.709964652185));
#18536=CARTESIAN_POINT('Ctrl Pts',(15.8,-8.4207653230234,-11.7174179347464));
#18537=CARTESIAN_POINT('Ctrl Pts',(15.8,-8.4252346384098,-11.7248463432757));
#18538=CARTESIAN_POINT('Ctrl Pts',(15.8,-8.42973848206085,-11.7322498653003));
#18539=CARTESIAN_POINT('Ctrl Pts',(10.0502525316942,-6.33125817110613,-6.62239247796685));
#18540=CARTESIAN_POINT('Ctrl Pts',(11.9668350211294,-8.09084464143287,-7.25643163809036));
#18541=CARTESIAN_POINT('Ctrl Pts',(13.8834175105647,-9.85043111175961,-7.89047079821388));
#18542=CARTESIAN_POINT('Ctrl Pts',(15.8,-11.6100175820864,-8.5245099583374));
#18543=CARTESIAN_POINT('Ctrl Pts',(10.0502525316942,-6.42803507865412,-6.74536016772823));
#18544=CARTESIAN_POINT('Ctrl Pts',(11.9668350211294,-8.21671225999593,-7.39344597705571));
#18545=CARTESIAN_POINT('Ctrl Pts',(13.8834175105647,-10.0057987839539,-8.04138429933134));
#18546=CARTESIAN_POINT('Ctrl Pts',(15.8,-11.7944759652957,-8.68947010865881));
#18547=CARTESIAN_POINT('Ctrl Pts',(10.0502525316942,-6.65988565896848,-6.95639005916883));
#18548=CARTESIAN_POINT('Ctrl Pts',(11.9668350211295,-8.51136454012837,-7.62236086025714));
#18549=CARTESIAN_POINT('Ctrl Pts',(13.8834175105647,-10.3629488876586,-8.28779124445879));
#18550=CARTESIAN_POINT('Ctrl Pts',(15.8,-12.2144277688185,-8.9537620455471));
#18551=CARTESIAN_POINT('Ctrl Pts',(10.0502525316941,-7.2071677757859,-7.17140112925234));
#18552=CARTESIAN_POINT('Ctrl Pts',(11.9668350211294,-9.17886046565844,-7.82602495118037));
#18553=CARTESIAN_POINT('Ctrl Pts',(13.8834175105647,-11.1506718004078,-8.48103967091341));
#18554=CARTESIAN_POINT('Ctrl Pts',(15.8,-13.1223644902804,-9.13566349284145));
#18555=CARTESIAN_POINT('Ctrl Pts',(10.0502525316942,-7.64992225296746,-7.2512189308223));
#18556=CARTESIAN_POINT('Ctrl Pts',(11.9668350211294,-9.70870355968973,-7.88043377854937));
#18557=CARTESIAN_POINT('Ctrl Pts',(13.8834175105647,-11.7676943247925,-8.50859598070372));
#18558=CARTESIAN_POINT('Ctrl Pts',(15.8,-13.8264756315148,-9.13781082843079));
#18559=CARTESIAN_POINT('Ctrl Pts',(10.0502525316942,-7.92891439885425,-7.2752703501265));
#18560=CARTESIAN_POINT('Ctrl Pts',(11.9668350211294,-10.0398646795257,-7.88323296009842));
#18561=CARTESIAN_POINT('Ctrl Pts',(13.8834175105647,-12.1508149601973,-8.49119557007034));
#18562=CARTESIAN_POINT('Ctrl Pts',(15.8,-14.2617652408688,-9.09915818004226));
#18563=CARTESIAN_POINT('',(10.0502525316942,-7.92891439885425,-7.2752703501265));
#18564=CARTESIAN_POINT('',(15.8,-11.6100175820864,-8.5245099583374));
#18565=CARTESIAN_POINT('Ctrl Pts',(15.8,-11.6100175820864,-8.5245099583374));
#18566=CARTESIAN_POINT('Ctrl Pts',(15.548617675428,-11.3837844012199,-8.44542381127114));
#18567=CARTESIAN_POINT('Ctrl Pts',(15.2955013981404,-11.1556103968132,-8.36553547761193));
#18568=CARTESIAN_POINT('Ctrl Pts',(15.0417459576101,-10.9263572847363,-8.2850797017454));
#18569=CARTESIAN_POINT('Ctrl Pts',(14.7869004713563,-10.6961193804757,-8.20427831565579));
#18570=CARTESIAN_POINT('Ctrl Pts',(14.5314103188166,-10.4647929695835,-8.1229048237753));
#18571=CARTESIAN_POINT('Ctrl Pts',(14.2763844586684,-10.2332972079334,-8.04122266692363));
#18572=CARTESIAN_POINT('Ctrl Pts',(14.0169022052127,-9.99775622450725,-7.95811317318572));
#18573=CARTESIAN_POINT('Ctrl Pts',(13.7579006122711,-9.76203981941543,-7.87468439208691));
#18574=CARTESIAN_POINT('Ctrl Pts',(13.5005477950648,-9.52716576583561,-7.79123671760531));
#18575=CARTESIAN_POINT('Ctrl Pts',(13.3099967765756,-9.35325863471441,-7.72944979203118));
#18576=CARTESIAN_POINT('Ctrl Pts',(13.1203496703585,-9.17981437027969,-7.66765301700902));
#18577=CARTESIAN_POINT('Ctrl Pts',(12.9320806449423,-9.00726329348628,-7.605974791296));
#18578=CARTESIAN_POINT('Ctrl Pts',(12.7398364200678,-8.83106889328649,-7.54299426293974));
#18579=CARTESIAN_POINT('Ctrl Pts',(12.5465417638457,-8.65356006118371,-7.47935703277431));
#18580=CARTESIAN_POINT('Ctrl Pts',(12.3528702390452,-8.47524825078831,-7.41514339569057));
#18581=CARTESIAN_POINT('Ctrl Pts',(12.1588880967135,-8.29665045733786,-7.35082677040841));
#18582=CARTESIAN_POINT('Ctrl Pts',(11.9645278759626,-8.11724699610012,-7.2859321298648));
#18583=CARTESIAN_POINT('Ctrl Pts',(11.7704663856167,-7.93760110830991,-7.22055811872365));
#18584=CARTESIAN_POINT('Ctrl Pts',(11.5758138300786,-7.75740806182779,-7.15498499387686));
#18585=CARTESIAN_POINT('Ctrl Pts',(11.3814618274404,-7.57697105649318,-7.08892983490284));
#18586=CARTESIAN_POINT('Ctrl Pts',(11.1880933895777,-7.3969093635474,-7.02250642528026));
#18587=CARTESIAN_POINT('Ctrl Pts',(10.9918668985605,-7.21418629579192,-6.95510125442768));
#18588=CARTESIAN_POINT('Ctrl Pts',(10.7966532620501,-7.03184966122232,-6.88731709712114));
#18589=CARTESIAN_POINT('Ctrl Pts',(10.6031662272204,-6.85059991984825,-6.81928375787452));
#18590=CARTESIAN_POINT('Ctrl Pts',(10.4170524040783,-6.67625706354084,-6.75384296552654));
#18591=CARTESIAN_POINT('Ctrl Pts',(10.2325360986482,-6.50292032538269,-6.6881718401968));
#18592=CARTESIAN_POINT('Ctrl Pts',(10.0502525316942,-6.33125817110613,-6.62239247796685));
#18593=CARTESIAN_POINT('Ctrl Pts',(15.8,-11.6100175820864,-8.5245099583374));
#18594=CARTESIAN_POINT('Ctrl Pts',(15.8,-11.6164882582397,-8.53029664958107));
#18595=CARTESIAN_POINT('Ctrl Pts',(15.8,-11.6229840657775,-8.53604902696561));
#18596=CARTESIAN_POINT('Ctrl Pts',(15.8,-11.6295050046841,-8.54176709053684));
#18597=CARTESIAN_POINT('Ctrl Pts',(15.8,-11.6360510806824,-8.54745083246671));
#18598=CARTESIAN_POINT('Ctrl Pts',(15.8,-11.642622304659,-8.55310023610356));
#18599=CARTESIAN_POINT('Ctrl Pts',(10.0502525316942,-8.06781615908999,-4.34180314898733));
#18600=CARTESIAN_POINT('Ctrl Pts',(11.9668350211294,-9.93721121325641,-4.40106810140592));
#18601=CARTESIAN_POINT('Ctrl Pts',(13.8834175105647,-11.8066062674228,-4.46033305382451));
#18602=CARTESIAN_POINT('Ctrl Pts',(15.8,-13.6760013215893,-4.51959800624309));
#18603=CARTESIAN_POINT('Ctrl Pts',(10.0502525316942,-8.19785557353568,-4.4288466625333));
#18604=CARTESIAN_POINT('Ctrl Pts',(11.9668350211294,-10.0992581912947,-4.49248124812732));
#18605=CARTESIAN_POINT('Ctrl Pts',(13.8834175105647,-12.0010045410108,-4.55584907137464));
#18606=CARTESIAN_POINT('Ctrl Pts',(15.8,-13.9024071587698,-4.61948365696866));
#18607=CARTESIAN_POINT('Ctrl Pts',(10.0502525316942,-8.48356457498288,-4.55790932427762));
#18608=CARTESIAN_POINT('Ctrl Pts',(11.9668350211294,-10.4502219249867,-4.61914675531024));
#18609=CARTESIAN_POINT('Ctrl Pts',(13.8834175105647,-12.416810143598,-4.67984453466858));
#18610=CARTESIAN_POINT('Ctrl Pts',(15.8,-14.3834674936017,-4.74108196570119));
#18611=CARTESIAN_POINT('Ctrl Pts',(10.0502525316941,-9.07050287838801,-4.59327853800037));
#18612=CARTESIAN_POINT('Ctrl Pts',(11.9668350211294,-11.1479839451212,-4.60657624071161));
#18613=CARTESIAN_POINT('Ctrl Pts',(13.8834175105647,-13.2256962639304,-4.62021662092401));
#18614=CARTESIAN_POINT('Ctrl Pts',(15.8,-15.3031773306636,-4.63351432363524));
#18615=CARTESIAN_POINT('Ctrl Pts',(10.0502525316942,-9.51625828739342,-4.5323630334273));
#18616=CARTESIAN_POINT('Ctrl Pts',(11.9668350211294,-11.668713745839,-4.49458350302914));
#18617=CARTESIAN_POINT('Ctrl Pts',(13.8834175105647,-13.8210431256713,-4.45573812100054));
#18618=CARTESIAN_POINT('Ctrl Pts',(15.8,-15.9734985841168,-4.41795859060238));
#18619=CARTESIAN_POINT('Ctrl Pts',(10.0502525316942,-9.78902788303806,-4.46902397810655));
#18620=CARTESIAN_POINT('Ctrl Pts',(11.9668350211294,-11.9845316814717,-4.39491126897609));
#18621=CARTESIAN_POINT('Ctrl Pts',(13.8834175105647,-14.1800354799052,-4.32079855984563));
#18622=CARTESIAN_POINT('Ctrl Pts',(15.8,-16.3755392783388,-4.24668585071518));
#18623=CARTESIAN_POINT('',(10.0502525316942,-9.78902788303806,-4.46902397810655));
#18624=CARTESIAN_POINT('',(15.8,-13.6760013215893,-4.51959800624309));
#18625=CARTESIAN_POINT('Ctrl Pts',(15.8,-13.6760013215893,-4.51959800624309));
#18626=CARTESIAN_POINT('Ctrl Pts',(15.5486181428671,-13.4364022627901,-4.51429251817173));
#18627=CARTESIAN_POINT('Ctrl Pts',(15.2955023394669,-13.1947094870246,-4.50882385781796));
#18628=CARTESIAN_POINT('Ctrl Pts',(15.0417473731653,-12.9518150706355,-4.50314899406863));
#18629=CARTESIAN_POINT('Ctrl Pts',(14.7869020465168,-12.7078769606235,-4.49744974598312));
#18630=CARTESIAN_POINT('Ctrl Pts',(14.5314120523244,-12.4627268269498,-4.49154276300943));
#18631=CARTESIAN_POINT('Ctrl Pts',(14.2763863472133,-12.2173202460879,-4.4853945547262));
#18632=CARTESIAN_POINT('Ctrl Pts',(14.0169034957054,-11.9676246346078,-4.47913889270852));
#18633=CARTESIAN_POINT('Ctrl Pts',(13.7579013040845,-11.7176635180538,-4.4726337773552));
#18634=CARTESIAN_POINT('Ctrl Pts',(13.5005478956174,-11.468497691795,-4.46585038850012));
#18635=CARTESIAN_POINT('Ctrl Pts',(13.3099968432927,-11.2840089349537,-4.46082779372524));
#18636=CARTESIAN_POINT('Ctrl Pts',(13.1203497034746,-11.0999573476229,-4.45565279642647));
#18637=CARTESIAN_POINT('Ctrl Pts',(12.9320806449423,-10.9167918673754,-4.45031453415308));
#18638=CARTESIAN_POINT('Ctrl Pts',(12.7398361468872,-10.7297587134111,-4.44486355054889));
#18639=CARTESIAN_POINT('Ctrl Pts',(12.5465412144993,-10.5412725252547,-4.43919418585342));
#18640=CARTESIAN_POINT('Ctrl Pts',(12.3528694134191,-10.3518445394597,-4.4332247563449));
#18641=CARTESIAN_POINT('Ctrl Pts',(12.1588873388167,-10.162113078982,-4.42724576346213));
#18642=CARTESIAN_POINT('Ctrl Pts',(11.9645271870236,-9.97143676938872,-4.42096600829024));
#18643=CARTESIAN_POINT('Ctrl Pts',(11.7704657661437,-9.78038176737598,-4.41430525673783));
#18644=CARTESIAN_POINT('Ctrl Pts',(11.5758119966794,-9.58874359350202,-4.40762417406171));
#18645=CARTESIAN_POINT('Ctrl Pts',(11.3814587845902,-9.39672444179026,-4.4005600302801));
#18646=CARTESIAN_POINT('Ctrl Pts',(11.1880891545372,-9.2049484464285,-4.39302967416941));
#18647=CARTESIAN_POINT('Ctrl Pts',(10.9918593168758,-9.01033581554701,-4.38538793354691));
#18648=CARTESIAN_POINT('Ctrl Pts',(10.7966423735553,-8.81597360566181,-4.37726632301399));
#18649=CARTESIAN_POINT('Ctrl Pts',(10.6031521084283,-8.62256814054964,-4.36857183761347));
#18650=CARTESIAN_POINT('Ctrl Pts',(10.4170430723425,-8.43654066954415,-4.36020902775276));
#18651=CARTESIAN_POINT('Ctrl Pts',(10.2325314892389,-8.25139886794607,-4.35131627654662));
#18652=CARTESIAN_POINT('Ctrl Pts',(10.0502525316942,-8.06781615908999,-4.34180314898733));
#18653=CARTESIAN_POINT('Ctrl Pts',(15.8,-13.6760013215893,-4.51959800624309));
#18654=CARTESIAN_POINT('Ctrl Pts',(15.8,-13.6839434862452,-4.52310192776169));
#18655=CARTESIAN_POINT('Ctrl Pts',(15.8,-13.6918989487026,-4.52656544883607));
#18656=CARTESIAN_POINT('Ctrl Pts',(15.8,-13.6998677089605,-4.52998856951466));
#18657=CARTESIAN_POINT('Ctrl Pts',(15.8,-13.7078497700428,-4.53337128058405));
#18658=CARTESIAN_POINT('Ctrl Pts',(15.8,-13.7158451371576,-4.53671356284346));
#18659=CARTESIAN_POINT('Ctrl Pts',(10.0502525316942,-9.01464008964162,-1.6362078766636));
#18660=CARTESIAN_POINT('Ctrl Pts',(11.9668350211294,-10.8108543149047,-1.11489735491132));
#18661=CARTESIAN_POINT('Ctrl Pts',(13.8834175105647,-12.6070685401678,-0.593586833159037));
#18662=CARTESIAN_POINT('Ctrl Pts',(15.8,-14.4032827654308,-0.0722763114067561));
#18663=CARTESIAN_POINT('Ctrl Pts',(10.0502525316942,-9.16521284706123,-1.67880678842043));
#18664=CARTESIAN_POINT('Ctrl Pts',(11.9668350211294,-10.9932183651601,-1.15176115367482));
#18665=CARTESIAN_POINT('Ctrl Pts',(13.8834175105647,-12.8214683576781,-0.624355593844837));
#18666=CARTESIAN_POINT('Ctrl Pts',(15.8,-14.6494738757771,-0.0973099590992228));
#18667=CARTESIAN_POINT('Ctrl Pts',(10.0502525316942,-9.47681709721301,-1.71327315824378));
#18668=CARTESIAN_POINT('Ctrl Pts',(11.9668350211294,-11.3661427921348,-1.16378287280497));
#18669=CARTESIAN_POINT('Ctrl Pts',(13.8834175105647,-13.2552357701884,-0.613808798404411));
#18670=CARTESIAN_POINT('Ctrl Pts',(15.8,-15.1445614651102,-0.0643185129655956));
#18671=CARTESIAN_POINT('Ctrl Pts',(10.0502525316941,-10.0459586957056,-1.56553830329486));
#18672=CARTESIAN_POINT('Ctrl Pts',(11.9668350211294,-12.025869817826,-0.936208214997369));
#18673=CARTESIAN_POINT('Ctrl Pts',(13.8834175105647,-14.0061068566225,-0.307141231238407));
#18674=CARTESIAN_POINT('Ctrl Pts',(15.8,-15.9860179787428,0.322188857059084));
#18675=CARTESIAN_POINT('Ctrl Pts',(10.0502525316942,-10.4510766569791,-1.36984786349029));
#18676=CARTESIAN_POINT('Ctrl Pts',(11.9668350211294,-12.4865089298363,-0.668772078627758));
#18677=CARTESIAN_POINT('Ctrl Pts',(13.8834175105647,-14.5214919285394,0.0332784309391876));
#18678=CARTESIAN_POINT('Ctrl Pts',(15.8,-16.5569242013966,0.734354215801724));
#18679=CARTESIAN_POINT('Ctrl Pts',(10.0502525316942,-10.6909231138624,-1.22531840158854));
#18680=CARTESIAN_POINT('Ctrl Pts',(11.9668350211294,-12.7560692212929,-0.47638504169901));
#18681=CARTESIAN_POINT('Ctrl Pts',(13.8834175105647,-14.8212153287235,0.272548318190525));
#18682=CARTESIAN_POINT('Ctrl Pts',(15.8,-16.886361436154,1.02148167808006));
#18683=CARTESIAN_POINT('',(10.0502525316942,-10.6909231138624,-1.22531840158854));
#18684=CARTESIAN_POINT('',(15.8,-14.4032827654308,-0.0722763114067561));
#18685=CARTESIAN_POINT('Ctrl Pts',(15.8,-14.4032827654308,-0.0722763114067562));
#18686=CARTESIAN_POINT('Ctrl Pts',(15.5486186601033,-14.1737715055211,-0.14127053144869));
#18687=CARTESIAN_POINT('Ctrl Pts',(15.2955033810747,-13.9422185866337,-0.210756563075385));
#18688=CARTESIAN_POINT('Ctrl Pts',(15.0417489395224,-13.7094591215774,-0.280417814422079));
#18689=CARTESIAN_POINT('Ctrl Pts',(14.7869037890753,-13.4756991900176,-0.350378489676399));
#18690=CARTESIAN_POINT('Ctrl Pts',(14.5314139696904,-13.2407223608428,-0.420516137034358));
#18691=CARTESIAN_POINT('Ctrl Pts',(14.2763884357272,-13.0054270908218,-0.490503613096571));
#18692=CARTESIAN_POINT('Ctrl Pts',(14.016904922593,-12.7660187369206,-0.561714506695313));
#18693=CARTESIAN_POINT('Ctrl Pts',(13.7579020686534,-12.5262807827901,-0.632770201644789));
#18694=CARTESIAN_POINT('Ctrl Pts',(13.5005480060758,-12.2872132071331,-0.703315478824681));
#18695=CARTESIAN_POINT('Ctrl Pts',(13.3099969165823,-12.1102018689489,-0.755548885558621));
#18696=CARTESIAN_POINT('Ctrl Pts',(13.1203497398531,-11.9335592090237,-0.807502254261612));
#18697=CARTESIAN_POINT('Ctrl Pts',(12.9320806449423,-11.7577088361878,-0.859026524117213));
#18698=CARTESIAN_POINT('Ctrl Pts',(12.7398358447897,-11.5781450060298,-0.911638839304067));
#18699=CARTESIAN_POINT('Ctrl Pts',(12.5465406070029,-11.3971317706544,-0.964492472593927));
#18700=CARTESIAN_POINT('Ctrl Pts',(12.3528685003979,-11.2151301058934,-1.0173517555325));
#18701=CARTESIAN_POINT('Ctrl Pts',(12.1588865006943,-11.032837221809,-1.0702956181623));
#18702=CARTESIAN_POINT('Ctrl Pts',(11.9645264251583,-10.8495527946037,-1.1232454100055));
#18703=CARTESIAN_POINT('Ctrl Pts',(11.7704650810977,-10.6657904772718,-1.1759498724029));
#18704=CARTESIAN_POINT('Ctrl Pts',(11.5758099697569,-10.4814659044743,-1.22881559404254));
#18705=CARTESIAN_POINT('Ctrl Pts',(11.3814554207386,-10.296660622926,-1.28143472519609));
#18706=CARTESIAN_POINT('Ctrl Pts',(11.188084472837,-10.1119425360181,-1.33353531202339));
#18707=CARTESIAN_POINT('Ctrl Pts',(10.9918509346348,-9.92448995248781,-1.38640717621227));
#18708=CARTESIAN_POINT('Ctrl Pts',(10.7966303348196,-9.73712725458383,-1.43874524883732));
#18709=CARTESIAN_POINT('Ctrl Pts',(10.6031364978028,-9.55049749194704,-1.49024279648039));
#18710=CARTESIAN_POINT('Ctrl Pts',(10.4170327545865,-9.37099566409686,-1.53977350262891));
#18711=CARTESIAN_POINT('Ctrl Pts',(10.2325263927835,-9.19217237538483,-1.58852655489952));
#18712=CARTESIAN_POINT('Ctrl Pts',(10.0502525316942,-9.01464008964162,-1.6362078766636));
#18713=CARTESIAN_POINT('Ctrl Pts',(15.8,-14.4032827654308,-0.0722763114067561));
#18714=CARTESIAN_POINT('Ctrl Pts',(15.8,-14.4119189841766,-0.0731544749487809));
#18715=CARTESIAN_POINT('Ctrl Pts',(15.8,-14.4205553654592,-0.0739901061384699));
#18716=CARTESIAN_POINT('Ctrl Pts',(15.8,-14.4291919092927,-0.0747832050221164));
#18717=CARTESIAN_POINT('Ctrl Pts',(15.8,-14.437828615706,-0.075533761902827));
#18718=CARTESIAN_POINT('Ctrl Pts',(15.8,-14.4464654837189,-0.0762417569101975));
#18719=CARTESIAN_POINT('Ctrl Pts',(10.0502525316942,-9.07904823952839,1.22955082275859));
#18720=CARTESIAN_POINT('Ctrl Pts',(11.9668350211294,-10.626255672559,2.28040731262864));
#18721=CARTESIAN_POINT('Ctrl Pts',(13.8834175105647,-12.1734631055895,3.33126380249869));
#18722=CARTESIAN_POINT('Ctrl Pts',(15.8,-13.7206705386201,4.38212029236874));
#18723=CARTESIAN_POINT('Ctrl Pts',(10.0502525316942,-9.23541522932356,1.23556639107773));
#18724=CARTESIAN_POINT('Ctrl Pts',(11.9668350211294,-10.8110857311875,2.3017013472912));
#18725=CARTESIAN_POINT('Ctrl Pts',(13.8834175105647,-12.3868775190731,3.36825415935174));
#18726=CARTESIAN_POINT('Ctrl Pts',(15.8,-13.962548020937,4.43438911556521));
#18727=CARTESIAN_POINT('Ctrl Pts',(10.0502525316942,-9.54242006948552,1.29909254545998));
#18728=CARTESIAN_POINT('Ctrl Pts',(11.9668350211295,-11.1694737466002,2.40552260970754));
#18729=CARTESIAN_POINT('Ctrl Pts',(13.8834175105647,-12.7961532691502,3.51235208206865));
#18730=CARTESIAN_POINT('Ctrl Pts',(15.8,-14.4232069462649,4.61878214631621));
#18731=CARTESIAN_POINT('Ctrl Pts',(10.0502525316941,-10.0380523375239,1.61547231497529));
#18732=CARTESIAN_POINT('Ctrl Pts',(11.9668350211294,-11.7265860195463,2.82582698043838));
#18733=CARTESIAN_POINT('Ctrl Pts',(13.8834175105647,-13.4155069687334,4.03604403376327));
#18734=CARTESIAN_POINT('Ctrl Pts',(15.8,-15.1040406507558,5.24639869922637));
#18735=CARTESIAN_POINT('Ctrl Pts',(10.0502525316942,-10.3628708264468,1.92675755961641));
#18736=CARTESIAN_POINT('Ctrl Pts',(11.9668350211294,-12.0820376211579,3.22250341643877));
#18737=CARTESIAN_POINT('Ctrl Pts',(13.8834175105647,-13.8004759242586,4.51903745819409));
#18738=CARTESIAN_POINT('Ctrl Pts',(15.8,-15.5196427189696,5.81478331501644));
#18739=CARTESIAN_POINT('Ctrl Pts',(10.0502525316942,-10.5463163022605,2.13832987737225));
#18740=CARTESIAN_POINT('Ctrl Pts',(11.9668350211294,-12.2789538289737,3.48877307262933));
#18741=CARTESIAN_POINT('Ctrl Pts',(13.8834175105647,-14.0115913556869,4.8392162678864));
#18742=CARTESIAN_POINT('Ctrl Pts',(15.8,-15.7442288824001,6.18965946314348));
#18743=CARTESIAN_POINT('',(10.0502525316942,-10.5463163022605,2.13832987737225));
#18744=CARTESIAN_POINT('',(15.8,-13.7206705386201,4.38212029236874));
#18745=CARTESIAN_POINT('Ctrl Pts',(15.8,-13.7206705386201,4.38212029236874));
#18746=CARTESIAN_POINT('Ctrl Pts',(15.5486179127188,-13.5237121602491,4.24557960414927));
#18747=CARTESIAN_POINT('Ctrl Pts',(15.2955018759953,-13.3249640154789,4.10794026962892));
#18748=CARTESIAN_POINT('Ctrl Pts',(15.0417466762024,-13.1251225182499,3.96976145165588));
#18749=CARTESIAN_POINT('Ctrl Pts',(14.7869012710154,-12.9244224444146,3.83098897769929));
#18750=CARTESIAN_POINT('Ctrl Pts',(14.5314111989041,-12.7226197192336,3.69167215691717));
#18751=CARTESIAN_POINT('Ctrl Pts',(14.2763854175035,-12.5204677360903,3.55239975641101));
#18752=CARTESIAN_POINT('Ctrl Pts',(14.0169028604367,-12.3147829883989,3.41069346140935));
#18753=CARTESIAN_POINT('Ctrl Pts',(13.7579009635655,-12.1087368195384,3.26903291905499));
#18754=CARTESIAN_POINT('Ctrl Pts',(13.5005478461955,-11.9031704882057,3.12806496166625));
#18755=CARTESIAN_POINT('Ctrl Pts',(13.3099968105011,-11.7509637547506,3.02368856803765));
#18756=CARTESIAN_POINT('Ctrl Pts',(13.1203496871979,-11.5990211190179,2.91969243162133));
#18757=CARTESIAN_POINT('Ctrl Pts',(12.9320806449423,-11.4476993942222,2.81634921885376));
#18758=CARTESIAN_POINT('Ctrl Pts',(12.7398362813706,-11.2931824947396,2.71082390290206));
#18759=CARTESIAN_POINT('Ctrl Pts',(12.5465414849356,-11.1373617066508,2.60462118886905));
#18760=CARTESIAN_POINT('Ctrl Pts',(12.3528698198645,-10.9806026156662,2.49810765644051));
#18761=CARTESIAN_POINT('Ctrl Pts',(12.1588877119198,-10.8235922502236,2.39142338986218));
#18762=CARTESIAN_POINT('Ctrl Pts',(11.9645275261796,-10.6656407015685,2.28442707498227));
#18763=CARTESIAN_POINT('Ctrl Pts',(11.7704660711025,-10.5071588397369,2.17751640137267));
#18764=CARTESIAN_POINT('Ctrl Pts',(11.5758128991794,-10.3481937475419,2.07027974418963));
#18765=CARTESIAN_POINT('Ctrl Pts',(11.3814602824285,-10.1886952830851,1.96312905478025));
#18766=CARTESIAN_POINT('Ctrl Pts',(11.1880912392174,-10.0291195021212,1.85649845736387));
#18767=CARTESIAN_POINT('Ctrl Pts',(10.9918630490259,-9.86718424000812,1.74829122417604));
#18768=CARTESIAN_POINT('Ctrl Pts',(10.796647733566,-9.7051695117194,1.6406193963383));
#18769=CARTESIAN_POINT('Ctrl Pts',(10.6031590586342,-9.54359206502174,1.53397337210477));
#18770=CARTESIAN_POINT('Ctrl Pts',(10.4170476660419,-9.38817519823614,1.43139351779793));
#18771=CARTESIAN_POINT('Ctrl Pts',(10.2325337582961,-9.23316336539128,1.32976299718739));
#18772=CARTESIAN_POINT('Ctrl Pts',(10.0502525316942,-9.07904823952839,1.22955082275859));
#18773=CARTESIAN_POINT('Ctrl Pts',(15.8,-13.7206705386201,4.38212029236874));
#18774=CARTESIAN_POINT('Ctrl Pts',(15.8,-13.7291554381927,4.38395384756931));
#18775=CARTESIAN_POINT('Ctrl Pts',(15.8,-13.7376273491274,4.38582790366735));
#18776=CARTESIAN_POINT('Ctrl Pts',(15.8,-13.7460862714518,4.38774246062322));
#18777=CARTESIAN_POINT('Ctrl Pts',(15.8,-13.7545322021969,4.38969752766811));
#18778=CARTESIAN_POINT('Ctrl Pts',(15.8,-13.7629651342901,4.39169312339699));
#18779=CARTESIAN_POINT('Ctrl Pts',(10.0502525316942,-8.25473589028142,3.97495252086484));
#18780=CARTESIAN_POINT('Ctrl Pts',(11.9668350211294,-9.40148508750639,5.45248982387649));
#18781=CARTESIAN_POINT('Ctrl Pts',(13.8834175105647,-10.5482342847314,6.93002712688815));
#18782=CARTESIAN_POINT('Ctrl Pts',(15.8,-11.6949834819563,8.40756442989979));
#18783=CARTESIAN_POINT('Ctrl Pts',(10.0502525316942,-8.40159082201815,4.02899372351993));
#18784=CARTESIAN_POINT('Ctrl Pts',(11.9668350211294,-9.57068870058276,5.52985728348807));
#18785=CARTESIAN_POINT('Ctrl Pts',(13.8834175105647,-10.7397728044506,7.03115572742428));
#18786=CARTESIAN_POINT('Ctrl Pts',(15.8,-11.9088706830152,8.53201928739242));
#18787=CARTESIAN_POINT('Ctrl Pts',(10.0502525316942,-8.6739375870516,4.18428628311193));
#18788=CARTESIAN_POINT('Ctrl Pts',(11.9668350211294,-9.87945189609367,5.73935104252813));
#18789=CARTESIAN_POINT('Ctrl Pts',(13.8834175105647,-11.0844841840221,7.29468404041881));
#18790=CARTESIAN_POINT('Ctrl Pts',(15.8,-12.2899984930642,8.84974879983501));
#18791=CARTESIAN_POINT('Ctrl Pts',(10.0502525316941,-9.04754461221301,4.63834053369691));
#18792=CARTESIAN_POINT('Ctrl Pts',(11.9668350211294,-10.2794154126352,6.31124182863326));
#18793=CARTESIAN_POINT('Ctrl Pts',(13.8834175105647,-11.5116939035746,7.98413616433457));
#18794=CARTESIAN_POINT('Ctrl Pts',(15.8,-12.7435647039968,9.65703745927091));
#18795=CARTESIAN_POINT('Ctrl Pts',(10.0502525316942,-9.26027499705532,5.0347585282786));
#18796=CARTESIAN_POINT('Ctrl Pts',(11.9668350211294,-10.4948922896145,6.79833782460276));
#18797=CARTESIAN_POINT('Ctrl Pts',(13.8834175105647,-11.7285731829415,8.56244161305558));
#18798=CARTESIAN_POINT('Ctrl Pts',(15.8,-12.9631904755006,10.3260209093797));
#18799=CARTESIAN_POINT('Ctrl Pts',(10.0502525316942,-9.36936257048691,5.29266352931554));
#18800=CARTESIAN_POINT('Ctrl Pts',(11.9668350211294,-10.5998888833726,7.11242577089738));
#18801=CARTESIAN_POINT('Ctrl Pts',(13.8834175105647,-11.8304151962582,8.93218801247923));
#18802=CARTESIAN_POINT('Ctrl Pts',(15.8,-13.0609415091439,10.7519502540611));
#18803=CARTESIAN_POINT('',(10.0502525316942,-9.36936257048691,5.29266352931554));
#18804=CARTESIAN_POINT('',(15.8,-11.6949834819563,8.40756442989979));
#18805=CARTESIAN_POINT('Ctrl Pts',(15.8,-11.6949834819563,8.40756442989979));
#18806=CARTESIAN_POINT('Ctrl Pts',(15.5486176029467,-11.5498581470169,8.2168427975067));
#18807=CARTESIAN_POINT('Ctrl Pts',(15.2955012521777,-11.4033701387264,8.02452322133705));
#18808=CARTESIAN_POINT('Ctrl Pts',(15.0417457381132,-11.2560089976705,7.83135270226922));
#18809=CARTESIAN_POINT('Ctrl Pts',(14.7869002270809,-11.1080148725492,7.63735242672965));
#18810=CARTESIAN_POINT('Ctrl Pts',(14.5314100499576,-10.9591402752378,7.44249371079261));
#18811=CARTESIAN_POINT('Ctrl Pts',(14.2763841657393,-10.8099197880111,7.24756931575076));
#18812=CARTESIAN_POINT('Ctrl Pts',(14.0169020050296,-10.6580918487946,7.04923884684354));
#18813=CARTESIAN_POINT('Ctrl Pts',(13.7579005049311,-10.5059060414972,6.85084020761523));
#18814=CARTESIAN_POINT('Ctrl Pts',(13.5005477794176,-10.3539625665109,6.65324852970321));
#18815=CARTESIAN_POINT('Ctrl Pts',(13.3099967661937,-10.2414594521427,6.50694623445595));
#18816=CARTESIAN_POINT('Ctrl Pts',(13.1203496652052,-10.1290900041786,6.36108719500196));
#18817=CARTESIAN_POINT('Ctrl Pts',(12.9320806449423,-10.0171093135792,6.21604099337274));
#18818=CARTESIAN_POINT('Ctrl Pts',(12.7398364624423,-9.9027642328537,6.06793224761101));
#18819=CARTESIAN_POINT('Ctrl Pts',(12.5465418490578,-9.78738841037966,5.9187763350222));
#18820=CARTESIAN_POINT('Ctrl Pts',(12.3528703671126,-9.67121625884623,5.76903486398374));
#18821=CARTESIAN_POINT('Ctrl Pts',(12.158888214275,-9.55485775408393,5.61905319074316));
#18822=CARTESIAN_POINT('Ctrl Pts',(11.9645279828276,-9.43770055909667,5.46848389786716));
#18823=CARTESIAN_POINT('Ctrl Pts',(11.7704664817064,-9.32001254164074,5.31783217681239));
#18824=CARTESIAN_POINT('Ctrl Pts',(11.5758141145071,-9.20196619521732,5.16672176100839));
#18825=CARTESIAN_POINT('Ctrl Pts',(11.3814622995134,-9.08338602074636,5.01552828296821));
#18826=CARTESIAN_POINT('Ctrl Pts',(11.1880940466173,-8.96457159711279,4.86480554216884));
#18827=CARTESIAN_POINT('Ctrl Pts',(10.9918680747392,-8.84400125838633,4.71185532487866));
#18828=CARTESIAN_POINT('Ctrl Pts',(10.7966549511887,-8.72318989748022,4.55938973719232));
#18829=CARTESIAN_POINT('Ctrl Pts',(10.6031684174502,-8.60247741697948,4.40803483977044));
#18830=CARTESIAN_POINT('Ctrl Pts',(10.4170538516981,-8.48636416374598,4.26244666645502));
#18831=CARTESIAN_POINT('Ctrl Pts',(10.2325368136997,-8.37034275782459,4.11788655117379));
#18832=CARTESIAN_POINT('Ctrl Pts',(10.0502525316942,-8.25473589028142,3.97495252086484));
#18833=CARTESIAN_POINT('Ctrl Pts',(15.8,-11.6949834819563,8.40756442989979));
#18834=CARTESIAN_POINT('Ctrl Pts',(15.8,-11.7024865012679,8.41193022268479));
#18835=CARTESIAN_POINT('Ctrl Pts',(15.8,-11.709964652185,8.41633052040236));
#18836=CARTESIAN_POINT('Ctrl Pts',(15.8,-11.7174179347464,8.4207653230234));
#18837=CARTESIAN_POINT('Ctrl Pts',(15.8,-11.7248463432757,8.4252346384098));
#18838=CARTESIAN_POINT('Ctrl Pts',(15.8,-11.7322498653003,8.42973848206085));
#18839=CARTESIAN_POINT('Ctrl Pts',(10.0502525316942,-6.62239247796685,6.33125817110613));
#18840=CARTESIAN_POINT('Ctrl Pts',(11.9668350211294,-7.25643163809036,8.09084464143287));
#18841=CARTESIAN_POINT('Ctrl Pts',(13.8834175105647,-7.89047079821388,9.85043111175961));
#18842=CARTESIAN_POINT('Ctrl Pts',(15.8,-8.5245099583374,11.6100175820864));
#18843=CARTESIAN_POINT('Ctrl Pts',(10.0502525316942,-6.74536016772823,6.42803507865412));
#18844=CARTESIAN_POINT('Ctrl Pts',(11.9668350211294,-7.39344597705571,8.21671225999593));
#18845=CARTESIAN_POINT('Ctrl Pts',(13.8834175105647,-8.04138429933134,10.0057987839539));
#18846=CARTESIAN_POINT('Ctrl Pts',(15.8,-8.68947010865881,11.7944759652957));
#18847=CARTESIAN_POINT('Ctrl Pts',(10.0502525316942,-6.95639005916883,6.65988565896847));
#18848=CARTESIAN_POINT('Ctrl Pts',(11.9668350211295,-7.62236086025714,8.51136454012837));
#18849=CARTESIAN_POINT('Ctrl Pts',(13.8834175105647,-8.28779124445879,10.3629488876586));
#18850=CARTESIAN_POINT('Ctrl Pts',(15.8,-8.9537620455471,12.2144277688185));
#18851=CARTESIAN_POINT('Ctrl Pts',(10.0502525316941,-7.17140112925234,7.2071677757859));
#18852=CARTESIAN_POINT('Ctrl Pts',(11.9668350211294,-7.82602495118037,9.17886046565844));
#18853=CARTESIAN_POINT('Ctrl Pts',(13.8834175105647,-8.48103967091341,11.1506718004078));
#18854=CARTESIAN_POINT('Ctrl Pts',(15.8,-9.13566349284145,13.1223644902804));
#18855=CARTESIAN_POINT('Ctrl Pts',(10.0502525316942,-7.2512189308223,7.64992225296746));
#18856=CARTESIAN_POINT('Ctrl Pts',(11.9668350211294,-7.88043377854937,9.70870355968973));
#18857=CARTESIAN_POINT('Ctrl Pts',(13.8834175105647,-8.50859598070372,11.7676943247925));
#18858=CARTESIAN_POINT('Ctrl Pts',(15.8,-9.13781082843079,13.8264756315148));
#18859=CARTESIAN_POINT('Ctrl Pts',(10.0502525316942,-7.2752703501265,7.92891439885425));
#18860=CARTESIAN_POINT('Ctrl Pts',(11.9668350211294,-7.88323296009842,10.0398646795257));
#18861=CARTESIAN_POINT('Ctrl Pts',(13.8834175105647,-8.49119557007034,12.1508149601973));
#18862=CARTESIAN_POINT('Ctrl Pts',(15.8,-9.09915818004226,14.2617652408688));
#18863=CARTESIAN_POINT('',(10.0502525316942,-7.2752703501265,7.92891439885425));
#18864=CARTESIAN_POINT('',(15.8,-8.5245099583374,11.6100175820864));
#18865=CARTESIAN_POINT('Ctrl Pts',(15.8,-8.5245099583374,11.6100175820864));
#18866=CARTESIAN_POINT('Ctrl Pts',(15.5486176754281,-8.44542381127117,11.38378440122));
#18867=CARTESIAN_POINT('Ctrl Pts',(15.2955013981405,-8.36553547761197,11.1556103968133));
#18868=CARTESIAN_POINT('Ctrl Pts',(15.0417459576102,-8.28507970174545,10.9263572847364));
#18869=CARTESIAN_POINT('Ctrl Pts',(14.7869004713576,-8.20427831565622,10.6961193804769));
#18870=CARTESIAN_POINT('Ctrl Pts',(14.5314103188191,-8.12290482377611,10.4647929695858));
#18871=CARTESIAN_POINT('Ctrl Pts',(14.2763844586721,-8.04122266692482,10.2332972079368));
#18872=CARTESIAN_POINT('Ctrl Pts',(14.0169022052159,-7.95811317318675,9.99775622451016));
#18873=CARTESIAN_POINT('Ctrl Pts',(13.7579006122738,-7.87468439208777,9.76203981941787));
#18874=CARTESIAN_POINT('Ctrl Pts',(13.5005477950669,-7.79123671760601,9.52716576583757));
#18875=CARTESIAN_POINT('Ctrl Pts',(13.309996776577,-7.72944979203165,9.35325863471571));
#18876=CARTESIAN_POINT('Ctrl Pts',(13.1203496703592,-7.66765301700925,9.17981437028034));
#18877=CARTESIAN_POINT('Ctrl Pts',(12.9320806449423,-7.60597479129601,9.00726329348628));
#18878=CARTESIAN_POINT('Ctrl Pts',(12.739836420068,-7.5429942629398,8.83106889328666));
#18879=CARTESIAN_POINT('Ctrl Pts',(12.5465417638461,-7.47935703277444,8.65356006118405));
#18880=CARTESIAN_POINT('Ctrl Pts',(12.3528702390458,-7.41514339569077,8.47524825078884));
#18881=CARTESIAN_POINT('Ctrl Pts',(12.158888096714,-7.35082677040859,8.29665045733833));
#18882=CARTESIAN_POINT('Ctrl Pts',(11.9645278759631,-7.28593212986495,8.11724699610054));
#18883=CARTESIAN_POINT('Ctrl Pts',(11.7704663856171,-7.22055811872379,7.93760110831027));
#18884=CARTESIAN_POINT('Ctrl Pts',(11.5758138300791,-7.15498499387704,7.75740806182827));
#18885=CARTESIAN_POINT('Ctrl Pts',(11.381461827441,-7.08892983490307,7.57697105649378));
#18886=CARTESIAN_POINT('Ctrl Pts',(11.1880933895784,-7.02250642528054,7.39690936354813));
#18887=CARTESIAN_POINT('Ctrl Pts',(10.9918668985614,-6.95510125442799,7.21418629579277));
#18888=CARTESIAN_POINT('Ctrl Pts',(10.7966532620511,-6.8873170971215,7.03184966122329));
#18889=CARTESIAN_POINT('Ctrl Pts',(10.6031662272216,-6.81928375787493,6.85059991984934));
#18890=CARTESIAN_POINT('Ctrl Pts',(10.417052404079,-6.75384296552681,6.67625706354156));
#18891=CARTESIAN_POINT('Ctrl Pts',(10.2325360986486,-6.68817184019694,6.50292032538305));
#18892=CARTESIAN_POINT('Ctrl Pts',(10.0502525316942,-6.62239247796685,6.33125817110613));
#18893=CARTESIAN_POINT('Ctrl Pts',(15.8,-8.5245099583374,11.6100175820864));
#18894=CARTESIAN_POINT('Ctrl Pts',(15.8,-8.53029664958107,11.6164882582397));
#18895=CARTESIAN_POINT('Ctrl Pts',(15.8,-8.53604902696561,11.6229840657775));
#18896=CARTESIAN_POINT('Ctrl Pts',(15.8,-8.54176709053684,11.6295050046841));
#18897=CARTESIAN_POINT('Ctrl Pts',(15.8,-8.54745083246671,11.6360510806824));
#18898=CARTESIAN_POINT('Ctrl Pts',(15.8,-8.55310023610356,11.642622304659));
#18899=CARTESIAN_POINT('Ctrl Pts',(10.0502525316942,-4.34180314898733,8.06781615908999));
#18900=CARTESIAN_POINT('Ctrl Pts',(11.9668350211294,-4.40106810140592,9.93721121325641));
#18901=CARTESIAN_POINT('Ctrl Pts',(13.8834175105647,-4.46033305382451,11.8066062674228));
#18902=CARTESIAN_POINT('Ctrl Pts',(15.8,-4.51959800624309,13.6760013215893));
#18903=CARTESIAN_POINT('Ctrl Pts',(10.0502525316942,-4.4288466625333,8.19785557353568));
#18904=CARTESIAN_POINT('Ctrl Pts',(11.9668350211294,-4.49248124812732,10.0992581912947));
#18905=CARTESIAN_POINT('Ctrl Pts',(13.8834175105647,-4.55584907137465,12.0010045410108));
#18906=CARTESIAN_POINT('Ctrl Pts',(15.8,-4.61948365696867,13.9024071587698));
#18907=CARTESIAN_POINT('Ctrl Pts',(10.0502525316942,-4.55790932427761,8.48356457498288));
#18908=CARTESIAN_POINT('Ctrl Pts',(11.9668350211294,-4.61914675531023,10.4502219249867));
#18909=CARTESIAN_POINT('Ctrl Pts',(13.8834175105647,-4.67984453466858,12.416810143598));
#18910=CARTESIAN_POINT('Ctrl Pts',(15.8,-4.7410819657012,14.3834674936017));
#18911=CARTESIAN_POINT('Ctrl Pts',(10.0502525316941,-4.59327853800039,9.07050287838801));
#18912=CARTESIAN_POINT('Ctrl Pts',(11.9668350211294,-4.60657624071163,11.1479839451212));
#18913=CARTESIAN_POINT('Ctrl Pts',(13.8834175105647,-4.62021662092399,13.2256962639304));
#18914=CARTESIAN_POINT('Ctrl Pts',(15.8,-4.63351432363522,15.3031773306636));
#18915=CARTESIAN_POINT('Ctrl Pts',(10.0502525316942,-4.53236303342729,9.51625828739342));
#18916=CARTESIAN_POINT('Ctrl Pts',(11.9668350211294,-4.49458350302913,11.668713745839));
#18917=CARTESIAN_POINT('Ctrl Pts',(13.8834175105647,-4.45573812100054,13.8210431256713));
#18918=CARTESIAN_POINT('Ctrl Pts',(15.8,-4.41795859060238,15.9734985841168));
#18919=CARTESIAN_POINT('Ctrl Pts',(10.0502525316942,-4.46902397810655,9.78902788303806));
#18920=CARTESIAN_POINT('Ctrl Pts',(11.9668350211294,-4.39491126897609,11.9845316814717));
#18921=CARTESIAN_POINT('Ctrl Pts',(13.8834175105647,-4.32079855984564,14.1800354799052));
#18922=CARTESIAN_POINT('Ctrl Pts',(15.8,-4.24668585071518,16.3755392783388));
#18923=CARTESIAN_POINT('',(10.0502525316942,-4.46902397810655,9.78902788303806));
#18924=CARTESIAN_POINT('',(15.8,-4.51959800624309,13.6760013215893));
#18925=CARTESIAN_POINT('Ctrl Pts',(15.8,-4.51959800624309,13.6760013215893));
#18926=CARTESIAN_POINT('Ctrl Pts',(15.5486181428668,-4.51429251817173,13.4364022627899));
#18927=CARTESIAN_POINT('Ctrl Pts',(15.2955023394664,-4.50882385781795,13.1947094870241));
#18928=CARTESIAN_POINT('Ctrl Pts',(15.0417473731645,-4.50314899406862,12.9518150706348));
#18929=CARTESIAN_POINT('Ctrl Pts',(14.7869020465161,-4.49744974598311,12.7078769606229));
#18930=CARTESIAN_POINT('Ctrl Pts',(14.531412052324,-4.49154276300942,12.4627268269494));
#18931=CARTESIAN_POINT('Ctrl Pts',(14.276386347213,-4.4853945547262,12.2173202460876));
#18932=CARTESIAN_POINT('Ctrl Pts',(14.0169034957048,-4.4791388927085,11.9676246346072));
#18933=CARTESIAN_POINT('Ctrl Pts',(13.7579013040838,-4.47263377735518,11.717663518053));
#18934=CARTESIAN_POINT('Ctrl Pts',(13.5005478956164,-4.46585038850009,11.468497691794));
#18935=CARTESIAN_POINT('Ctrl Pts',(13.309996843292,-4.46082779372523,11.2840089349531));
#18936=CARTESIAN_POINT('Ctrl Pts',(13.1203497034743,-4.45565279642646,11.0999573476226));
#18937=CARTESIAN_POINT('Ctrl Pts',(12.9320806449423,-4.45031453415308,10.9167918673754));
#18938=CARTESIAN_POINT('Ctrl Pts',(12.7398361468868,-4.44486355054888,10.7297587134107));
#18939=CARTESIAN_POINT('Ctrl Pts',(12.5465412144983,-4.43919418585339,10.5412725252538));
#18940=CARTESIAN_POINT('Ctrl Pts',(12.3528694134176,-4.43322475634486,10.3518445394583));
#18941=CARTESIAN_POINT('Ctrl Pts',(12.1588873388154,-4.42724576346209,10.1621130789808));
#18942=CARTESIAN_POINT('Ctrl Pts',(11.9645271870224,-4.4209660082902,9.97143676938756));
#18943=CARTESIAN_POINT('Ctrl Pts',(11.7704657661427,-4.41430525673779,9.78038176737493));
#18944=CARTESIAN_POINT('Ctrl Pts',(11.5758119966785,-4.40762417406168,9.58874359350119));
#18945=CARTESIAN_POINT('Ctrl Pts',(11.3814587845896,-4.40056003028007,9.39672444178965));
#18946=CARTESIAN_POINT('Ctrl Pts',(11.1880891545368,-4.39302967416939,9.2049484464281));
#18947=CARTESIAN_POINT('Ctrl Pts',(10.9918593168755,-4.3853879335469,9.01033581554672));
#18948=CARTESIAN_POINT('Ctrl Pts',(10.7966423735551,-4.37726632301398,8.81597360566162));
#18949=CARTESIAN_POINT('Ctrl Pts',(10.6031521084282,-4.36857183761346,8.62256814054954));
#18950=CARTESIAN_POINT('Ctrl Pts',(10.4170430723424,-4.36020902775276,8.43654066954408));
#18951=CARTESIAN_POINT('Ctrl Pts',(10.2325314892389,-4.35131627654661,8.25139886794604));
#18952=CARTESIAN_POINT('Ctrl Pts',(10.0502525316942,-4.34180314898733,8.06781615908999));
#18953=CARTESIAN_POINT('Ctrl Pts',(15.8,-4.51959800624309,13.6760013215893));
#18954=CARTESIAN_POINT('Ctrl Pts',(15.8,-4.52310192776169,13.6839434862452));
#18955=CARTESIAN_POINT('Ctrl Pts',(15.8,-4.52656544883607,13.6918989487026));
#18956=CARTESIAN_POINT('Ctrl Pts',(15.8,-4.52998856951466,13.6998677089605));
#18957=CARTESIAN_POINT('Ctrl Pts',(15.8,-4.53337128058405,13.7078497700428));
#18958=CARTESIAN_POINT('Ctrl Pts',(15.8,-4.53671356284346,13.7158451371576));
#18959=CARTESIAN_POINT('Ctrl Pts',(10.0502525316942,-1.6362078766636,9.01464008964162));
#18960=CARTESIAN_POINT('Ctrl Pts',(11.9668350211294,-1.11489735491132,10.8108543149047));
#18961=CARTESIAN_POINT('Ctrl Pts',(13.8834175105647,-0.593586833159038,
12.6070685401678));
#18962=CARTESIAN_POINT('Ctrl Pts',(15.8,-0.072276311406757,14.4032827654308));
#18963=CARTESIAN_POINT('Ctrl Pts',(10.0502525316942,-1.67880678842043,9.16521284706123));
#18964=CARTESIAN_POINT('Ctrl Pts',(11.9668350211294,-1.15176115367482,10.9932183651601));
#18965=CARTESIAN_POINT('Ctrl Pts',(13.8834175105647,-0.624355593844837,
12.8214683576781));
#18966=CARTESIAN_POINT('Ctrl Pts',(15.8,-0.0973099590992238,14.6494738757771));
#18967=CARTESIAN_POINT('Ctrl Pts',(10.0502525316942,-1.71327315824378,9.47681709721301));
#18968=CARTESIAN_POINT('Ctrl Pts',(11.9668350211294,-1.16378287280496,11.3661427921348));
#18969=CARTESIAN_POINT('Ctrl Pts',(13.8834175105647,-0.613808798404414,
13.2552357701884));
#18970=CARTESIAN_POINT('Ctrl Pts',(15.8,-0.064318512965597,15.1445614651102));
#18971=CARTESIAN_POINT('Ctrl Pts',(10.0502525316941,-1.56553830329486,10.0459586957056));
#18972=CARTESIAN_POINT('Ctrl Pts',(11.9668350211294,-0.936208214997367,
12.025869817826));
#18973=CARTESIAN_POINT('Ctrl Pts',(13.8834175105647,-0.307141231238408,
14.0061068566225));
#18974=CARTESIAN_POINT('Ctrl Pts',(15.8,0.322188857059081,15.9860179787428));
#18975=CARTESIAN_POINT('Ctrl Pts',(10.0502525316942,-1.36984786349029,10.4510766569791));
#18976=CARTESIAN_POINT('Ctrl Pts',(11.9668350211294,-0.668772078627758,
12.4865089298363));
#18977=CARTESIAN_POINT('Ctrl Pts',(13.8834175105647,0.0332784309391854,
14.5214919285394));
#18978=CARTESIAN_POINT('Ctrl Pts',(15.8,0.734354215801722,16.5569242013966));
#18979=CARTESIAN_POINT('Ctrl Pts',(10.0502525316942,-1.22531840158854,10.6909231138624));
#18980=CARTESIAN_POINT('Ctrl Pts',(11.9668350211294,-0.47638504169901,12.7560692212929));
#18981=CARTESIAN_POINT('Ctrl Pts',(13.8834175105647,0.272548318190524,14.8212153287235));
#18982=CARTESIAN_POINT('Ctrl Pts',(15.8,1.02148167808006,16.886361436154));
#18983=CARTESIAN_POINT('',(10.0502525316942,-1.22531840158854,10.6909231138624));
#18984=CARTESIAN_POINT('',(15.8,-0.072276311406757,14.4032827654308));
#18985=CARTESIAN_POINT('Ctrl Pts',(15.8,-0.0722763114067571,14.4032827654308));
#18986=CARTESIAN_POINT('Ctrl Pts',(15.5486186601032,-0.141270531448724,
14.173771505521));
#18987=CARTESIAN_POINT('Ctrl Pts',(15.2955033810745,-0.210756563075445,
13.9422185866335));
#18988=CARTESIAN_POINT('Ctrl Pts',(15.0417489395221,-0.28041781442216,13.7094591215771));
#18989=CARTESIAN_POINT('Ctrl Pts',(14.7869037890755,-0.350378489676339,
13.4756991900178));
#18990=CARTESIAN_POINT('Ctrl Pts',(14.5314139696912,-0.420516137034151,
13.2407223608434));
#18991=CARTESIAN_POINT('Ctrl Pts',(14.2763884357285,-0.490503613096215,
13.005427090823));
#18992=CARTESIAN_POINT('Ctrl Pts',(14.0169049225932,-0.561714506695251,
12.7660187369208));
#18993=CARTESIAN_POINT('Ctrl Pts',(13.7579020686526,-0.632770201645017,
12.5262807827893));
#18994=CARTESIAN_POINT('Ctrl Pts',(13.5005480060739,-0.703315478825194,
12.2872132071314));
#18995=CARTESIAN_POINT('Ctrl Pts',(13.3099969165811,-0.755548885558961,
12.1102018689477));
#18996=CARTESIAN_POINT('Ctrl Pts',(13.1203497398525,-0.807502254261781,
11.9335592090231));
#18997=CARTESIAN_POINT('Ctrl Pts',(12.9320806449423,-0.859026524117214,
11.7577088361878));
#18998=CARTESIAN_POINT('Ctrl Pts',(12.7398358447895,-0.911638839304132,
11.5781450060296));
#18999=CARTESIAN_POINT('Ctrl Pts',(12.5465406070024,-0.964492472594062,
11.397131770654));
#19000=CARTESIAN_POINT('Ctrl Pts',(12.3528685003971,-1.0173517555327,11.2151301058927));
#19001=CARTESIAN_POINT('Ctrl Pts',(12.1588865006936,-1.07029561816249,11.0328372218084));
#19002=CARTESIAN_POINT('Ctrl Pts',(11.9645264251577,-1.12324541000567,10.8495527946032));
#19003=CARTESIAN_POINT('Ctrl Pts',(11.7704650810972,-1.17594987240305,10.6657904772713));
#19004=CARTESIAN_POINT('Ctrl Pts',(11.5758099697562,-1.22881559404272,10.4814659044737));
#19005=CARTESIAN_POINT('Ctrl Pts',(11.3814554207379,-1.28143472519631,10.2966606229252));
#19006=CARTESIAN_POINT('Ctrl Pts',(11.1880844728361,-1.33353531202364,10.1119425360172));
#19007=CARTESIAN_POINT('Ctrl Pts',(10.991850934634,-1.38640717621249,9.92448995248705));
#19008=CARTESIAN_POINT('Ctrl Pts',(10.796630334819,-1.4387452488375,9.73712725458319));
#19009=CARTESIAN_POINT('Ctrl Pts',(10.6031364978022,-1.49024279648053,9.55049749194653));
#19010=CARTESIAN_POINT('Ctrl Pts',(10.4170327545862,-1.539773502629,9.37099566409652));
#19011=CARTESIAN_POINT('Ctrl Pts',(10.2325263927833,-1.58852655489957,9.19217237538466));
#19012=CARTESIAN_POINT('Ctrl Pts',(10.0502525316942,-1.6362078766636,9.01464008964162));
#19013=CARTESIAN_POINT('Ctrl Pts',(15.8,-0.072276311406757,14.4032827654308));
#19014=CARTESIAN_POINT('Ctrl Pts',(15.8,-0.0731544749487818,14.4119189841766));
#19015=CARTESIAN_POINT('Ctrl Pts',(15.8,-0.0739901061384708,14.4205553654592));
#19016=CARTESIAN_POINT('Ctrl Pts',(15.8,-0.0747832050221173,14.4291919092927));
#19017=CARTESIAN_POINT('Ctrl Pts',(15.8,-0.0755337619028279,14.437828615706));
#19018=CARTESIAN_POINT('Ctrl Pts',(15.8,-0.0762417569101984,14.4464654837189));
#19019=CARTESIAN_POINT('Ctrl Pts',(10.0502525316942,1.22955082275859,9.07904823952839));
#19020=CARTESIAN_POINT('Ctrl Pts',(11.9668350211294,2.28040731262864,10.626255672559));
#19021=CARTESIAN_POINT('Ctrl Pts',(13.8834175105647,3.33126380249869,12.1734631055895));
#19022=CARTESIAN_POINT('Ctrl Pts',(15.8,4.38212029236874,13.7206705386201));
#19023=CARTESIAN_POINT('Ctrl Pts',(10.0502525316942,1.23556639107773,9.23541522932356));
#19024=CARTESIAN_POINT('Ctrl Pts',(11.9668350211294,2.3017013472912,10.8110857311875));
#19025=CARTESIAN_POINT('Ctrl Pts',(13.8834175105647,3.36825415935174,12.386877519073));
#19026=CARTESIAN_POINT('Ctrl Pts',(15.8,4.43438911556521,13.962548020937));
#19027=CARTESIAN_POINT('Ctrl Pts',(10.0502525316942,1.29909254545998,9.54242006948551));
#19028=CARTESIAN_POINT('Ctrl Pts',(11.9668350211295,2.40552260970754,11.1694737466002));
#19029=CARTESIAN_POINT('Ctrl Pts',(13.8834175105647,3.51235208206865,12.7961532691502));
#19030=CARTESIAN_POINT('Ctrl Pts',(15.8,4.61878214631621,14.4232069462649));
#19031=CARTESIAN_POINT('Ctrl Pts',(10.0502525316941,1.61547231497529,10.0380523375239));
#19032=CARTESIAN_POINT('Ctrl Pts',(11.9668350211294,2.82582698043838,11.7265860195464));
#19033=CARTESIAN_POINT('Ctrl Pts',(13.8834175105647,4.03604403376328,13.4155069687334));
#19034=CARTESIAN_POINT('Ctrl Pts',(15.8,5.24639869922637,15.1040406507558));
#19035=CARTESIAN_POINT('Ctrl Pts',(10.0502525316942,1.92675755961642,10.3628708264469));
#19036=CARTESIAN_POINT('Ctrl Pts',(11.9668350211294,3.22250341643878,12.0820376211579));
#19037=CARTESIAN_POINT('Ctrl Pts',(13.8834175105647,4.51903745819409,13.8004759242586));
#19038=CARTESIAN_POINT('Ctrl Pts',(15.8,5.81478331501644,15.5196427189696));
#19039=CARTESIAN_POINT('Ctrl Pts',(10.0502525316942,2.13832987737225,10.5463163022605));
#19040=CARTESIAN_POINT('Ctrl Pts',(11.9668350211294,3.48877307262933,12.2789538289737));
#19041=CARTESIAN_POINT('Ctrl Pts',(13.8834175105647,4.8392162678864,14.0115913556869));
#19042=CARTESIAN_POINT('Ctrl Pts',(15.8,6.18965946314348,15.7442288824001));
#19043=CARTESIAN_POINT('',(10.0502525316942,2.13832987737225,10.5463163022605));
#19044=CARTESIAN_POINT('',(15.8,4.38212029236874,13.7206705386201));
#19045=CARTESIAN_POINT('Ctrl Pts',(15.8,4.38212029236874,13.7206705386201));
#19046=CARTESIAN_POINT('Ctrl Pts',(15.54861791272,4.24557960414993,13.5237121602501));
#19047=CARTESIAN_POINT('Ctrl Pts',(15.2955018759977,4.10794026963023,13.3249640154808));
#19048=CARTESIAN_POINT('Ctrl Pts',(15.041746676206,3.96976145165784,13.1251225182527));
#19049=CARTESIAN_POINT('Ctrl Pts',(14.7869012710187,3.83098897770111,12.9244224444172));
#19050=CARTESIAN_POINT('Ctrl Pts',(14.5314111989072,3.69167215691884,12.722619719236));
#19051=CARTESIAN_POINT('Ctrl Pts',(14.2763854175063,3.55239975641252,12.5204677360925));
#19052=CARTESIAN_POINT('Ctrl Pts',(14.0169028604397,3.41069346141102,12.3147829884014));
#19053=CARTESIAN_POINT('Ctrl Pts',(13.7579009635688,3.26903291905679,12.1087368195411));
#19054=CARTESIAN_POINT('Ctrl Pts',(13.500547846199,3.12806496166819,11.9031704882085));
#19055=CARTESIAN_POINT('Ctrl Pts',(13.3099968105034,3.02368856803894,11.7509637547525));
#19056=CARTESIAN_POINT('Ctrl Pts',(13.1203496871991,2.91969243162197,11.5990211190189));
#19057=CARTESIAN_POINT('Ctrl Pts',(12.9320806449423,2.81634921885376,11.4476993942222));
#19058=CARTESIAN_POINT('Ctrl Pts',(12.7398362813703,2.71082390290191,11.2931824947394));
#19059=CARTESIAN_POINT('Ctrl Pts',(12.5465414849351,2.60462118886877,11.1373617066504));
#19060=CARTESIAN_POINT('Ctrl Pts',(12.3528698198637,2.49810765644009,10.9806026156656));
#19061=CARTESIAN_POINT('Ctrl Pts',(12.1588877119191,2.39142338986178,10.8235922502231));
#19062=CARTESIAN_POINT('Ctrl Pts',(11.9645275261789,2.28442707498191,10.665640701568));
#19063=CARTESIAN_POINT('Ctrl Pts',(11.7704660711019,2.17751640137234,10.5071588397364));
#19064=CARTESIAN_POINT('Ctrl Pts',(11.5758128991788,2.07027974418934,10.3481937475415));
#19065=CARTESIAN_POINT('Ctrl Pts',(11.381460282428,1.96312905477998,10.1886952830847));
#19066=CARTESIAN_POINT('Ctrl Pts',(11.188091239217,1.85649845736363,10.0291195021208));
#19067=CARTESIAN_POINT('Ctrl Pts',(10.9918630490254,1.74829122417577,9.86718424000771));
#19068=CARTESIAN_POINT('Ctrl Pts',(10.7966477335654,1.64061939633799,9.70516951171893));
#19069=CARTESIAN_POINT('Ctrl Pts',(10.6031590586335,1.53397337210443,9.54359206502122));
#19070=CARTESIAN_POINT('Ctrl Pts',(10.4170476660415,1.4313935177977,9.38817519823579));
#19071=CARTESIAN_POINT('Ctrl Pts',(10.2325337582959,1.32976299718728,9.23316336539111));
#19072=CARTESIAN_POINT('Ctrl Pts',(10.0502525316942,1.22955082275859,9.07904823952839));
#19073=CARTESIAN_POINT('Ctrl Pts',(15.8,4.38212029236874,13.7206705386201));
#19074=CARTESIAN_POINT('Ctrl Pts',(15.8,4.38395384756931,13.7291554381927));
#19075=CARTESIAN_POINT('Ctrl Pts',(15.8,4.38582790366735,13.7376273491274));
#19076=CARTESIAN_POINT('Ctrl Pts',(15.8,4.38774246062322,13.7460862714518));
#19077=CARTESIAN_POINT('Ctrl Pts',(15.8,4.38969752766811,13.7545322021969));
#19078=CARTESIAN_POINT('Ctrl Pts',(15.8,4.39169312339699,13.7629651342901));
#19079=CARTESIAN_POINT('Ctrl Pts',(10.0502525316942,3.97495252086484,8.25473589028142));
#19080=CARTESIAN_POINT('Ctrl Pts',(11.9668350211294,5.45248982387649,9.40148508750639));
#19081=CARTESIAN_POINT('Ctrl Pts',(13.8834175105647,6.93002712688814,10.5482342847314));
#19082=CARTESIAN_POINT('Ctrl Pts',(15.8,8.40756442989979,11.6949834819563));
#19083=CARTESIAN_POINT('Ctrl Pts',(10.0502525316942,4.02899372351994,8.40159082201815));
#19084=CARTESIAN_POINT('Ctrl Pts',(11.9668350211294,5.52985728348808,9.57068870058276));
#19085=CARTESIAN_POINT('Ctrl Pts',(13.8834175105647,7.03115572742427,10.7397728044506));
#19086=CARTESIAN_POINT('Ctrl Pts',(15.8,8.53201928739241,11.9088706830152));
#19087=CARTESIAN_POINT('Ctrl Pts',(10.0502525316942,4.18428628311196,8.6739375870516));
#19088=CARTESIAN_POINT('Ctrl Pts',(11.9668350211294,5.73935104252815,9.87945189609366));
#19089=CARTESIAN_POINT('Ctrl Pts',(13.8834175105647,7.2946840404188,11.0844841840221));
#19090=CARTESIAN_POINT('Ctrl Pts',(15.8,8.84974879983499,12.2899984930642));
#19091=CARTESIAN_POINT('Ctrl Pts',(10.0502525316941,4.63834053369693,9.04754461221299));
#19092=CARTESIAN_POINT('Ctrl Pts',(11.9668350211294,6.31124182863328,10.2794154126352));
#19093=CARTESIAN_POINT('Ctrl Pts',(13.8834175105647,7.98413616433457,11.5116939035747));
#19094=CARTESIAN_POINT('Ctrl Pts',(15.8,9.65703745927091,12.7435647039969));
#19095=CARTESIAN_POINT('Ctrl Pts',(10.0502525316942,5.0347585282786,9.26027499705535));
#19096=CARTESIAN_POINT('Ctrl Pts',(11.9668350211294,6.79833782460276,10.4948922896145));
#19097=CARTESIAN_POINT('Ctrl Pts',(13.8834175105647,8.56244161305558,11.7285731829415));
#19098=CARTESIAN_POINT('Ctrl Pts',(15.8,10.3260209093797,12.9631904755006));
#19099=CARTESIAN_POINT('Ctrl Pts',(10.0502525316942,5.29266352931554,9.36936257048691));
#19100=CARTESIAN_POINT('Ctrl Pts',(11.9668350211294,7.11242577089738,10.5998888833726));
#19101=CARTESIAN_POINT('Ctrl Pts',(13.8834175105647,8.93218801247923,11.8304151962582));
#19102=CARTESIAN_POINT('Ctrl Pts',(15.8,10.7519502540611,13.0609415091439));
#19103=CARTESIAN_POINT('',(10.0502525316942,5.29266352931554,9.36936257048691));
#19104=CARTESIAN_POINT('',(15.8,8.40756442989979,11.6949834819563));
#19105=CARTESIAN_POINT('Ctrl Pts',(15.8,8.40756442989979,11.6949834819563));
#19106=CARTESIAN_POINT('Ctrl Pts',(15.5486176029462,8.21684279750629,11.5498581470166));
#19107=CARTESIAN_POINT('Ctrl Pts',(15.2955012521766,8.02452322133619,11.4033701387258));
#19108=CARTESIAN_POINT('Ctrl Pts',(15.0417457381114,7.83135270226788,11.2560089976695));
#19109=CARTESIAN_POINT('Ctrl Pts',(14.7869002270796,7.63735242672867,11.1080148725485));
#19110=CARTESIAN_POINT('Ctrl Pts',(14.5314100499567,7.44249371079197,10.9591402752373));
#19111=CARTESIAN_POINT('Ctrl Pts',(14.2763841657389,7.24756931575045,10.8099197880109));
#19112=CARTESIAN_POINT('Ctrl Pts',(14.0169020050304,7.04923884684417,10.6580918487951));
#19113=CARTESIAN_POINT('Ctrl Pts',(13.7579005049332,6.8508402076168,10.5059060414984));
#19114=CARTESIAN_POINT('Ctrl Pts',(13.5005477794209,6.6532485297057,10.3539625665128));
#19115=CARTESIAN_POINT('Ctrl Pts',(13.3099967661958,6.50694623445761,10.241459452144));
#19116=CARTESIAN_POINT('Ctrl Pts',(13.1203496652063,6.36108719500278,10.1290900041793));
#19117=CARTESIAN_POINT('Ctrl Pts',(12.9320806449423,6.21604099337274,10.0171093135792));
#19118=CARTESIAN_POINT('Ctrl Pts',(12.7398364624423,6.06793224761099,9.90276423285369));
#19119=CARTESIAN_POINT('Ctrl Pts',(12.5465418490578,5.91877633502217,9.78738841037964));
#19120=CARTESIAN_POINT('Ctrl Pts',(12.3528703671126,5.76903486398371,9.6712162588462));
#19121=CARTESIAN_POINT('Ctrl Pts',(12.158888214275,5.61905319074313,9.5548577540839));
#19122=CARTESIAN_POINT('Ctrl Pts',(11.9645279828276,5.46848389786713,9.43770055909665));
#19123=CARTESIAN_POINT('Ctrl Pts',(11.7704664817064,5.31783217681237,9.32001254164072));
#19124=CARTESIAN_POINT('Ctrl Pts',(11.5758141145067,5.16672176100811,9.20196619521711));
#19125=CARTESIAN_POINT('Ctrl Pts',(11.3814622995127,5.01552828296769,9.08338602074594));
#19126=CARTESIAN_POINT('Ctrl Pts',(11.1880940466163,4.86480554216807,8.96457159711218));
#19127=CARTESIAN_POINT('Ctrl Pts',(10.9918680747382,4.71185532487785,8.84400125838568));
#19128=CARTESIAN_POINT('Ctrl Pts',(10.7966549511876,4.55938973719146,8.72318989747954));
#19129=CARTESIAN_POINT('Ctrl Pts',(10.603168417449,4.40803483976955,8.60247741697877));
#19130=CARTESIAN_POINT('Ctrl Pts',(10.4170538516974,4.26244666645443,8.48636416374551));
#19131=CARTESIAN_POINT('Ctrl Pts',(10.2325368136993,4.1178865511735,8.37034275782436));
#19132=CARTESIAN_POINT('Ctrl Pts',(10.0502525316942,3.97495252086484,8.25473589028142));
#19133=CARTESIAN_POINT('Ctrl Pts',(15.8,8.40756442989979,11.6949834819563));
#19134=CARTESIAN_POINT('Ctrl Pts',(15.8,8.41193022268479,11.7024865012679));
#19135=CARTESIAN_POINT('Ctrl Pts',(15.8,8.41633052040235,11.709964652185));
#19136=CARTESIAN_POINT('Ctrl Pts',(15.8,8.4207653230234,11.7174179347465));
#19137=CARTESIAN_POINT('Ctrl Pts',(15.8,8.4252346384098,11.7248463432758));
#19138=CARTESIAN_POINT('Ctrl Pts',(15.8,8.42973848206085,11.7322498653004));
#19139=CARTESIAN_POINT('Ctrl Pts',(10.0502525316942,6.33125817110613,6.62239247796685));
#19140=CARTESIAN_POINT('Ctrl Pts',(11.9668350211294,8.09084464143287,7.25643163809036));
#19141=CARTESIAN_POINT('Ctrl Pts',(13.8834175105647,9.85043111175961,7.89047079821388));
#19142=CARTESIAN_POINT('Ctrl Pts',(15.8,11.6100175820863,8.5245099583374));
#19143=CARTESIAN_POINT('Ctrl Pts',(10.0502525316942,6.42803507865412,6.74536016772823));
#19144=CARTESIAN_POINT('Ctrl Pts',(11.9668350211294,8.21671225999592,7.39344597705571));
#19145=CARTESIAN_POINT('Ctrl Pts',(13.8834175105647,10.0057987839539,8.04138429933134));
#19146=CARTESIAN_POINT('Ctrl Pts',(15.8,11.7944759652957,8.68947010865881));
#19147=CARTESIAN_POINT('Ctrl Pts',(10.0502525316942,6.65988565896844,6.95639005916882));
#19148=CARTESIAN_POINT('Ctrl Pts',(11.9668350211295,8.51136454012834,7.62236086025713));
#19149=CARTESIAN_POINT('Ctrl Pts',(13.8834175105647,10.3629488876587,8.28779124445879));
#19150=CARTESIAN_POINT('Ctrl Pts',(15.8,12.2144277688186,8.9537620455471));
#19151=CARTESIAN_POINT('Ctrl Pts',(10.0502525316941,7.20716777578592,7.17140112925233));
#19152=CARTESIAN_POINT('Ctrl Pts',(11.9668350211294,9.17886046565845,7.82602495118037));
#19153=CARTESIAN_POINT('Ctrl Pts',(13.8834175105647,11.1506718004079,8.48103967091341));
#19154=CARTESIAN_POINT('Ctrl Pts',(15.8,13.1223644902804,9.13566349284145));
#19155=CARTESIAN_POINT('Ctrl Pts',(10.0502525316942,7.64992225296743,7.2512189308223));
#19156=CARTESIAN_POINT('Ctrl Pts',(11.9668350211294,9.70870355968971,7.88043377854937));
#19157=CARTESIAN_POINT('Ctrl Pts',(13.8834175105647,11.7676943247925,8.50859598070372));
#19158=CARTESIAN_POINT('Ctrl Pts',(15.8,13.8264756315148,9.13781082843079));
#19159=CARTESIAN_POINT('Ctrl Pts',(10.0502525316942,7.92891439885425,7.2752703501265));
#19160=CARTESIAN_POINT('Ctrl Pts',(11.9668350211294,10.0398646795257,7.88323296009842));
#19161=CARTESIAN_POINT('Ctrl Pts',(13.8834175105647,12.1508149601973,8.49119557007034));
#19162=CARTESIAN_POINT('Ctrl Pts',(15.8,14.2617652408688,9.09915818004226));
#19163=CARTESIAN_POINT('',(10.0502525316942,7.92891439885425,7.2752703501265));
#19164=CARTESIAN_POINT('',(15.8,11.6100175820863,8.5245099583374));
#19165=CARTESIAN_POINT('Ctrl Pts',(15.8,11.6100175820863,8.5245099583374));
#19166=CARTESIAN_POINT('Ctrl Pts',(15.548617675428,11.3837844012199,8.44542381127114));
#19167=CARTESIAN_POINT('Ctrl Pts',(15.2955013981403,11.1556103968132,8.36553547761191));
#19168=CARTESIAN_POINT('Ctrl Pts',(15.0417459576099,10.9263572847362,8.28507970174537));
#19169=CARTESIAN_POINT('Ctrl Pts',(14.786900471357,10.6961193804763,8.20427831565601));
#19170=CARTESIAN_POINT('Ctrl Pts',(14.5314103188181,10.4647929695849,8.12290482377579));
#19171=CARTESIAN_POINT('Ctrl Pts',(14.2763844586707,10.2332972079355,8.04122266692438));
#19172=CARTESIAN_POINT('Ctrl Pts',(14.0169022052158,9.99775622451002,7.9581131731867));
#19173=CARTESIAN_POINT('Ctrl Pts',(13.7579006122748,9.76203981941886,7.87468439208812));
#19174=CARTESIAN_POINT('Ctrl Pts',(13.5005477950692,9.52716576583967,7.79123671760675));
#19175=CARTESIAN_POINT('Ctrl Pts',(13.3099967765785,9.35325863471711,7.72944979203215));
#19176=CARTESIAN_POINT('Ctrl Pts',(13.1203496703599,9.17981437028103,7.6676530170095));
#19177=CARTESIAN_POINT('Ctrl Pts',(12.9320806449423,9.00726329348628,7.605974791296));
#19178=CARTESIAN_POINT('Ctrl Pts',(12.7398364200685,8.83106889328712,7.54299426293996));
#19179=CARTESIAN_POINT('Ctrl Pts',(12.5465417638471,8.65356006118498,7.47935703277477));
#19180=CARTESIAN_POINT('Ctrl Pts',(12.3528702390473,8.47524825079023,7.41514339569127));
#19181=CARTESIAN_POINT('Ctrl Pts',(12.1588880967154,8.29665045733962,7.35082677040905));
#19182=CARTESIAN_POINT('Ctrl Pts',(11.9645278759643,8.11724699610171,7.28593212986538));
#19183=CARTESIAN_POINT('Ctrl Pts',(11.7704663856183,7.93760110831134,7.22055811872417));
#19184=CARTESIAN_POINT('Ctrl Pts',(11.5758138300802,7.75740806182931,7.15498499387742));
#19185=CARTESIAN_POINT('Ctrl Pts',(11.3814618274421,7.57697105649479,7.08892983490344));
#19186=CARTESIAN_POINT('Ctrl Pts',(11.1880933895795,7.39690936354911,7.0225064252809));
#19187=CARTESIAN_POINT('Ctrl Pts',(10.9918668985623,7.21418629579357,6.95510125442829));
#19188=CARTESIAN_POINT('Ctrl Pts',(10.7966532620518,7.03184966122392,6.88731709712173));
#19189=CARTESIAN_POINT('Ctrl Pts',(10.6031662272221,6.85059991984979,6.8192837578751));
#19190=CARTESIAN_POINT('Ctrl Pts',(10.4170524040794,6.67625706354185,6.75384296552693));
#19191=CARTESIAN_POINT('Ctrl Pts',(10.2325360986488,6.50292032538319,6.68817184019699));
#19192=CARTESIAN_POINT('Ctrl Pts',(10.0502525316942,6.33125817110613,6.62239247796685));
#19193=CARTESIAN_POINT('Ctrl Pts',(15.8,11.6100175820863,8.5245099583374));
#19194=CARTESIAN_POINT('Ctrl Pts',(15.8,11.6164882582397,8.53029664958107));
#19195=CARTESIAN_POINT('Ctrl Pts',(15.8,11.6229840657775,8.53604902696561));
#19196=CARTESIAN_POINT('Ctrl Pts',(15.8,11.6295050046841,8.54176709053684));
#19197=CARTESIAN_POINT('Ctrl Pts',(15.8,11.6360510806824,8.54745083246671));
#19198=CARTESIAN_POINT('Ctrl Pts',(15.8,11.642622304659,8.55310023610356));
#19199=CARTESIAN_POINT('Ctrl Pts',(10.0502525316942,8.06781615908999,4.34180314898733));
#19200=CARTESIAN_POINT('Ctrl Pts',(11.9668350211294,9.93721121325641,4.40106810140592));
#19201=CARTESIAN_POINT('Ctrl Pts',(13.8834175105647,11.8066062674228,4.46033305382451));
#19202=CARTESIAN_POINT('Ctrl Pts',(15.8,13.6760013215893,4.51959800624309));
#19203=CARTESIAN_POINT('Ctrl Pts',(10.0502525316942,8.19785557353568,4.4288466625333));
#19204=CARTESIAN_POINT('Ctrl Pts',(11.9668350211294,10.0992581912947,4.49248124812732));
#19205=CARTESIAN_POINT('Ctrl Pts',(13.8834175105647,12.0010045410108,4.55584907137465));
#19206=CARTESIAN_POINT('Ctrl Pts',(15.8,13.9024071587698,4.61948365696866));
#19207=CARTESIAN_POINT('Ctrl Pts',(10.0502525316942,8.48356457498289,4.55790932427761));
#19208=CARTESIAN_POINT('Ctrl Pts',(11.9668350211294,10.4502219249867,4.61914675531023));
#19209=CARTESIAN_POINT('Ctrl Pts',(13.8834175105647,12.416810143598,4.67984453466857));
#19210=CARTESIAN_POINT('Ctrl Pts',(15.8,14.3834674936017,4.74108196570119));
#19211=CARTESIAN_POINT('Ctrl Pts',(10.0502525316941,9.07050287838801,4.59327853800039));
#19212=CARTESIAN_POINT('Ctrl Pts',(11.9668350211294,11.1479839451212,4.60657624071163));
#19213=CARTESIAN_POINT('Ctrl Pts',(13.8834175105647,13.2256962639304,4.62021662092402));
#19214=CARTESIAN_POINT('Ctrl Pts',(15.8,15.3031773306636,4.63351432363526));
#19215=CARTESIAN_POINT('Ctrl Pts',(10.0502525316942,9.51625828739344,4.53236303342729));
#19216=CARTESIAN_POINT('Ctrl Pts',(11.9668350211294,11.668713745839,4.49458350302913));
#19217=CARTESIAN_POINT('Ctrl Pts',(13.8834175105647,13.8210431256712,4.45573812100054));
#19218=CARTESIAN_POINT('Ctrl Pts',(15.8,15.9734985841168,4.41795859060239));
#19219=CARTESIAN_POINT('Ctrl Pts',(10.0502525316942,9.78902788303806,4.46902397810655));
#19220=CARTESIAN_POINT('Ctrl Pts',(11.9668350211294,11.9845316814717,4.39491126897609));
#19221=CARTESIAN_POINT('Ctrl Pts',(13.8834175105647,14.1800354799052,4.32079855984564));
#19222=CARTESIAN_POINT('Ctrl Pts',(15.8,16.3755392783388,4.24668585071518));
#19223=CARTESIAN_POINT('',(10.0502525316942,9.78902788303806,4.46902397810655));
#19224=CARTESIAN_POINT('',(15.8,13.6760013215893,4.51959800624309));
#19225=CARTESIAN_POINT('Ctrl Pts',(15.8,13.6760013215893,4.51959800624309));
#19226=CARTESIAN_POINT('Ctrl Pts',(15.5486181428676,13.4364022627906,4.51429251817174));
#19227=CARTESIAN_POINT('Ctrl Pts',(15.2955023394679,13.1947094870255,4.50882385781798));
#19228=CARTESIAN_POINT('Ctrl Pts',(15.0417473731668,12.9518150706369,4.50314899406867));
#19229=CARTESIAN_POINT('Ctrl Pts',(14.7869020465191,12.7078769606257,4.49744974598318));
#19230=CARTESIAN_POINT('Ctrl Pts',(14.5314120523275,12.4627268269528,4.49154276300951));
#19231=CARTESIAN_POINT('Ctrl Pts',(14.2763863472172,12.2173202460916,4.4853945547263));
#19232=CARTESIAN_POINT('Ctrl Pts',(14.01690349571,11.9676246346122,4.47913889270863));
#19233=CARTESIAN_POINT('Ctrl Pts',(13.7579013040899,11.7176635180589,4.47263377735534));
#19234=CARTESIAN_POINT('Ctrl Pts',(13.5005478956234,11.4684976918008,4.46585038850028));
#19235=CARTESIAN_POINT('Ctrl Pts',(13.3099968432967,11.2840089349576,4.46082779372536));
#19236=CARTESIAN_POINT('Ctrl Pts',(13.1203497034766,11.0999573476248,4.45565279642653));
#19237=CARTESIAN_POINT('Ctrl Pts',(12.9320806449423,10.9167918673754,4.45031453415308));
#19238=CARTESIAN_POINT('Ctrl Pts',(12.7398361468874,10.7297587134113,4.4448635505489));
#19239=CARTESIAN_POINT('Ctrl Pts',(12.5465412144996,10.5412725252551,4.43919418585343));
#19240=CARTESIAN_POINT('Ctrl Pts',(12.3528694134196,10.3518445394602,4.43322475634492));
#19241=CARTESIAN_POINT('Ctrl Pts',(12.1588873388172,10.1621130789825,4.42724576346214));
#19242=CARTESIAN_POINT('Ctrl Pts',(11.964527187024,9.97143676938913,4.42096600829026));
#19243=CARTESIAN_POINT('Ctrl Pts',(11.7704657661441,9.78038176737634,4.41430525673784));
#19244=CARTESIAN_POINT('Ctrl Pts',(11.5758119966797,9.58874359350238,4.40762417406172));
#19245=CARTESIAN_POINT('Ctrl Pts',(11.3814587845906,9.39672444179062,4.40056003028011));
#19246=CARTESIAN_POINT('Ctrl Pts',(11.1880891545376,9.20494844642885,4.39302967416942));
#19247=CARTESIAN_POINT('Ctrl Pts',(10.9918593168763,9.01033581554755,4.38538793354694));
#19248=CARTESIAN_POINT('Ctrl Pts',(10.796642373556,8.81597360566253,4.37726632301402));
#19249=CARTESIAN_POINT('Ctrl Pts',(10.6031521084292,8.62256814055053,4.36857183761351));
#19250=CARTESIAN_POINT('Ctrl Pts',(10.4170430723431,8.43654066954474,4.36020902775279));
#19251=CARTESIAN_POINT('Ctrl Pts',(10.2325314892392,8.25139886794637,4.35131627654663));
#19252=CARTESIAN_POINT('Ctrl Pts',(10.0502525316942,8.06781615908999,4.34180314898733));
#19253=CARTESIAN_POINT('Ctrl Pts',(15.8,13.6760013215893,4.51959800624309));
#19254=CARTESIAN_POINT('Ctrl Pts',(15.8,13.6839434862452,4.52310192776169));
#19255=CARTESIAN_POINT('Ctrl Pts',(15.8,13.6918989487026,4.52656544883607));
#19256=CARTESIAN_POINT('Ctrl Pts',(15.8,13.6998677089605,4.52998856951466));
#19257=CARTESIAN_POINT('Ctrl Pts',(15.8,13.7078497700428,4.53337128058406));
#19258=CARTESIAN_POINT('Ctrl Pts',(15.8,13.7158451371576,4.53671356284346));
#19259=CARTESIAN_POINT('Ctrl Pts',(10.0502525316942,9.01464008964162,1.6362078766636));
#19260=CARTESIAN_POINT('Ctrl Pts',(11.9668350211294,10.8108543149047,1.11489735491132));
#19261=CARTESIAN_POINT('Ctrl Pts',(13.8834175105647,12.6070685401678,0.593586833159039));
#19262=CARTESIAN_POINT('Ctrl Pts',(15.8,14.4032827654308,0.0722763114067579));
#19263=CARTESIAN_POINT('Ctrl Pts',(10.0502525316942,9.16521284706123,1.67880678842043));
#19264=CARTESIAN_POINT('Ctrl Pts',(11.9668350211294,10.9932183651601,1.15176115367482));
#19265=CARTESIAN_POINT('Ctrl Pts',(13.8834175105647,12.8214683576781,0.624355593844838));
#19266=CARTESIAN_POINT('Ctrl Pts',(15.8,14.6494738757771,0.0973099590992247));
#19267=CARTESIAN_POINT('Ctrl Pts',(10.0502525316942,9.47681709721301,1.71327315824379));
#19268=CARTESIAN_POINT('Ctrl Pts',(11.9668350211294,11.3661427921348,1.16378287280497));
#19269=CARTESIAN_POINT('Ctrl Pts',(13.8834175105647,13.2552357701884,0.613808798404414));
#19270=CARTESIAN_POINT('Ctrl Pts',(15.8,15.1445614651102,0.0643185129655977));
#19271=CARTESIAN_POINT('Ctrl Pts',(10.0502525316941,10.0459586957056,1.56553830329485));
#19272=CARTESIAN_POINT('Ctrl Pts',(11.9668350211294,12.025869817826,0.936208214997364));
#19273=CARTESIAN_POINT('Ctrl Pts',(13.8834175105647,14.0061068566225,0.307141231238409));
#19274=CARTESIAN_POINT('Ctrl Pts',(15.8,15.9860179787428,-0.32218885705908));
#19275=CARTESIAN_POINT('Ctrl Pts',(10.0502525316942,10.4510766569791,1.3698478634903));
#19276=CARTESIAN_POINT('Ctrl Pts',(11.9668350211294,12.4865089298363,0.668772078627759));
#19277=CARTESIAN_POINT('Ctrl Pts',(13.8834175105647,14.5214919285394,-0.0332784309391845));
#19278=CARTESIAN_POINT('Ctrl Pts',(15.8,16.5569242013966,-0.734354215801722));
#19279=CARTESIAN_POINT('Ctrl Pts',(10.0502525316942,10.6909231138624,1.22531840158854));
#19280=CARTESIAN_POINT('Ctrl Pts',(11.9668350211294,12.7560692212929,0.476385041699011));
#19281=CARTESIAN_POINT('Ctrl Pts',(13.8834175105647,14.8212153287235,-0.272548318190523));
#19282=CARTESIAN_POINT('Ctrl Pts',(15.8,16.886361436154,-1.02148167808006));
#19283=CARTESIAN_POINT('',(10.0502525316942,10.6909231138624,1.22531840158854));
#19284=CARTESIAN_POINT('',(15.8,14.4032827654308,0.0722763114067579));
#19285=CARTESIAN_POINT('Ctrl Pts',(15.8,14.4032827654308,0.0722763114067579));
#19286=CARTESIAN_POINT('Ctrl Pts',(15.5486186601037,14.1737715055214,0.141270531448591));
#19287=CARTESIAN_POINT('Ctrl Pts',(15.2955033810755,13.9422185866344,0.210756563075182));
#19288=CARTESIAN_POINT('Ctrl Pts',(15.0417489395235,13.7094591215784,0.280417814421773));
#19289=CARTESIAN_POINT('Ctrl Pts',(14.7869037890761,13.4756991900184,0.350378489676167));
#19290=CARTESIAN_POINT('Ctrl Pts',(14.531413969691,13.2407223608433,0.4205161370342));
#19291=CARTESIAN_POINT('Ctrl Pts',(14.2763884357275,13.0054270908221,0.490503613096486));
#19292=CARTESIAN_POINT('Ctrl Pts',(14.0169049225932,12.7660187369208,0.56171450669525));
#19293=CARTESIAN_POINT('Ctrl Pts',(13.7579020686536,12.5262807827902,0.632770201644749));
#19294=CARTESIAN_POINT('Ctrl Pts',(13.5005480060759,12.2872132071332,0.703315478824662));
#19295=CARTESIAN_POINT('Ctrl Pts',(13.3099969165824,12.1102018689489,0.755548885558609));
#19296=CARTESIAN_POINT('Ctrl Pts',(13.1203497398532,11.9335592090237,0.807502254261607));
#19297=CARTESIAN_POINT('Ctrl Pts',(12.9320806449423,11.7577088361878,0.859026524117214));
#19298=CARTESIAN_POINT('Ctrl Pts',(12.7398358447892,11.5781450060293,0.911638839304226));
#19299=CARTESIAN_POINT('Ctrl Pts',(12.5465406070018,11.3971317706534,0.964492472594246));
#19300=CARTESIAN_POINT('Ctrl Pts',(12.3528685003961,11.2151301058918,1.01735175553297));
#19301=CARTESIAN_POINT('Ctrl Pts',(12.1588865006927,11.0328372218075,1.07029561816274));
#19302=CARTESIAN_POINT('Ctrl Pts',(11.9645264251569,10.8495527946024,1.1232454100059));
#19303=CARTESIAN_POINT('Ctrl Pts',(11.7704650810964,10.6657904772706,1.17594987240326));
#19304=CARTESIAN_POINT('Ctrl Pts',(11.5758099697556,10.4814659044731,1.2288155940429));
#19305=CARTESIAN_POINT('Ctrl Pts',(11.3814554207373,10.2966606229247,1.28143472519645));
#19306=CARTESIAN_POINT('Ctrl Pts',(11.1880844728357,10.1119425360169,1.33353531202374));
#19307=CARTESIAN_POINT('Ctrl Pts',(10.9918509346335,9.92448995248661,1.38640717621261));
#19308=CARTESIAN_POINT('Ctrl Pts',(10.7966303348184,9.73712725458267,1.43874524883765));
#19309=CARTESIAN_POINT('Ctrl Pts',(10.6031364978016,9.55049749194593,1.49024279648069));
#19310=CARTESIAN_POINT('Ctrl Pts',(10.4170327545858,9.37099566409612,1.53977350262911));
#19311=CARTESIAN_POINT('Ctrl Pts',(10.2325263927831,9.19217237538446,1.58852655489962));
#19312=CARTESIAN_POINT('Ctrl Pts',(10.0502525316942,9.01464008964162,1.6362078766636));
#19313=CARTESIAN_POINT('Ctrl Pts',(15.8,14.4032827654308,0.0722763114067579));
#19314=CARTESIAN_POINT('Ctrl Pts',(15.8,14.4119189841766,0.0731544749487826));
#19315=CARTESIAN_POINT('Ctrl Pts',(15.8,14.4205553654592,0.0739901061384717));
#19316=CARTESIAN_POINT('Ctrl Pts',(15.8,14.4291919092927,0.0747832050221182));
#19317=CARTESIAN_POINT('Ctrl Pts',(15.8,14.437828615706,0.0755337619028287));
#19318=CARTESIAN_POINT('Ctrl Pts',(15.8,14.4464654837189,0.0762417569101993));
#19319=CARTESIAN_POINT('Ctrl Pts',(10.0502525316942,10.5463163022605,-2.13832987737225));
#19320=CARTESIAN_POINT('Ctrl Pts',(11.9668350211294,12.2789538289737,-3.48877307262933));
#19321=CARTESIAN_POINT('Ctrl Pts',(13.8834175105647,14.0115913556869,-4.8392162678864));
#19322=CARTESIAN_POINT('Ctrl Pts',(15.8,15.7442288824001,-6.18965946314348));
#19323=CARTESIAN_POINT('Ctrl Pts',(10.0502525316942,10.4407180108925,-2.39160131057558));
#19324=CARTESIAN_POINT('Ctrl Pts',(11.9668350211294,12.1359573145141,-3.77416649083142));
#19325=CARTESIAN_POINT('Ctrl Pts',(13.8834175105647,13.8309364798931,-5.15732892266062));
#19326=CARTESIAN_POINT('Ctrl Pts',(15.8,15.5261757835147,-6.53989410291646));
#19327=CARTESIAN_POINT('Ctrl Pts',(10.0502525316942,10.2391038402362,-2.76042111194549));
#19328=CARTESIAN_POINT('Ctrl Pts',(11.9668350211294,11.8698223691572,-4.18872035504581));
#19329=CARTESIAN_POINT('Ctrl Pts',(13.8834175105647,13.5008577836237,-5.61629814839675));
#19330=CARTESIAN_POINT('Ctrl Pts',(15.8,15.1315763125447,-7.04459739149707));
#19331=CARTESIAN_POINT('Ctrl Pts',(10.0502525316942,10.0106660065973,-2.88380634898391));
#19332=CARTESIAN_POINT('Ctrl Pts',(11.9668350211294,11.5875472242667,-4.31947109051328));
#19333=CARTESIAN_POINT('Ctrl Pts',(13.8834175105647,13.1642822866715,-5.75550424110767));
#19334=CARTESIAN_POINT('Ctrl Pts',(15.8,14.7411635043409,-7.19116898263704));
#19335=CARTESIAN_POINT('Ctrl Pts',(10.0502525316942,9.83366631411429,-2.90441220847246));
#19336=CARTESIAN_POINT('Ctrl Pts',(11.9668350211294,11.3745625747195,-4.33027001363173));
#19337=CARTESIAN_POINT('Ctrl Pts',(13.8834175105647,12.9152995332973,-5.75638324902558));
#19338=CARTESIAN_POINT('Ctrl Pts',(15.8,14.4561957939025,-7.18224105418485));
#19339=CARTESIAN_POINT('Ctrl Pts',(10.0502525316941,9.65650945139357,-2.93414649567711));
#19340=CARTESIAN_POINT('Ctrl Pts',(11.9668350211294,11.1613433397504,-4.34899924292337));
#19341=CARTESIAN_POINT('Ctrl Pts',(13.8834175105647,12.6660861533134,-5.76416819477548));
#19342=CARTESIAN_POINT('Ctrl Pts',(15.8,14.1709200416702,-7.17902094202175));
#19343=CARTESIAN_POINT('Ctrl Pts',(10.0502525316942,9.38996734645582,-3.00074150798573));
#19344=CARTESIAN_POINT('Ctrl Pts',(11.9668350211294,10.8390518176275,-4.40343923355922));
#19345=CARTESIAN_POINT('Ctrl Pts',(13.8834175105647,12.2880463890101,-5.80619247524443));
#19346=CARTESIAN_POINT('Ctrl Pts',(15.8,13.7371308601818,-7.20889020081793));
#19347=CARTESIAN_POINT('Ctrl Pts',(10.0502525316942,9.13374448664767,-2.99092345166593));
#19348=CARTESIAN_POINT('Ctrl Pts',(11.9668350211294,10.5342467491227,-4.37002011593522));
#19349=CARTESIAN_POINT('Ctrl Pts',(13.8834175105647,11.9347028120052,-5.74920012742634));
#19350=CARTESIAN_POINT('Ctrl Pts',(15.8,13.3352050744803,-7.12829679169563));
#19351=CARTESIAN_POINT('Ctrl Pts',(10.0502525316942,8.89063737063807,-2.94970615383952));
#19352=CARTESIAN_POINT('Ctrl Pts',(11.9668350211294,10.2485256494886,-4.29832412978306));
#19353=CARTESIAN_POINT('Ctrl Pts',(13.8834175105647,11.6063785007713,-5.64703889510257));
#19354=CARTESIAN_POINT('Ctrl Pts',(15.8,12.9642667796218,-6.99565687104612));
#19355=CARTESIAN_POINT('Ctrl Pts',(10.0502525316942,8.77435756124985,-2.90932499072146));
#19356=CARTESIAN_POINT('Ctrl Pts',(11.9668350211294,10.113663592731,-4.23975104071156));
#19357=CARTESIAN_POINT('Ctrl Pts',(13.8834175105647,11.4529271015425,-5.57015841015681));
#19358=CARTESIAN_POINT('Ctrl Pts',(15.8,12.7922331330237,-6.90058446014691));
#19359=CARTESIAN_POINT('Ctrl Pts',(10.0502525316942,8.69919410795919,-2.87487982939776));
#19360=CARTESIAN_POINT('Ctrl Pts',(11.9668350211294,10.0272667966845,-4.19183584103558));
#19361=CARTESIAN_POINT('Ctrl Pts',(13.8834175105647,11.3553394854098,-5.5087918526734));
#19362=CARTESIAN_POINT('Ctrl Pts',(15.8,12.6834121741351,-6.82574786431123));
#19363=CARTESIAN_POINT('',(15.8,12.6834121741351,-6.82574786431123));
#19364=CARTESIAN_POINT('Ctrl Pts',(15.8,12.7194492253464,-6.84994811524973));
#19365=CARTESIAN_POINT('Ctrl Pts',(15.8,12.7121990649934,-6.84519519909218));
#19366=CARTESIAN_POINT('Ctrl Pts',(15.8,12.7049702849691,-6.84039870583253));
#19367=CARTESIAN_POINT('Ctrl Pts',(15.8,12.6977628786185,-6.83555864794507));
#19368=CARTESIAN_POINT('Ctrl Pts',(15.8,12.6905768416977,-6.83067503400497));
#19369=CARTESIAN_POINT('Ctrl Pts',(15.8,12.6834121741351,-6.82574786431123));
#19370=CARTESIAN_POINT('Ctrl Pts',(10.0502525316942,8.69919410795919,-2.87487982939776));
#19371=CARTESIAN_POINT('Ctrl Pts',(10.2643339107007,8.85499138412423,-3.02539831429572));
#19372=CARTESIAN_POINT('Ctrl Pts',(10.4809652372448,9.01135162140509,-3.17730962520325));
#19373=CARTESIAN_POINT('Ctrl Pts',(10.6991643144455,9.16765819773425,-3.32988591467729));
#19374=CARTESIAN_POINT('Ctrl Pts',(10.8996105956421,9.31124758570826,-3.47004851397053));
#19375=CARTESIAN_POINT('Ctrl Pts',(11.1013798991828,9.45479172976614,-3.61077172321218));
#19376=CARTESIAN_POINT('Ctrl Pts',(11.3037107883209,9.59785289528413,-3.75150991597921));
#19377=CARTESIAN_POINT('Ctrl Pts',(11.5002306637608,9.73680529423647,-3.88820605876814));
#19378=CARTESIAN_POINT('Ctrl Pts',(11.6972803301583,9.8753020317765,-4.02491580697293));
#19379=CARTESIAN_POINT('Ctrl Pts',(11.894162090759,10.0129819298195,-4.16116553050558));
#19380=CARTESIAN_POINT('Ctrl Pts',(12.0857947176331,10.146991095774,-4.29378265233427));
#19381=CARTESIAN_POINT('Ctrl Pts',(12.2772682725492,10.280226529135,-4.42596360023171));
#19382=CARTESIAN_POINT('Ctrl Pts',(12.4679393887634,10.4123927004731,-4.55730333099484));
#19383=CARTESIAN_POINT('Ctrl Pts',(12.6135640193747,10.5133343127246,-4.65761375113995));
#19384=CARTESIAN_POINT('Ctrl Pts',(12.7587205789995,10.6136529851627,-4.757434090911));
#19385=CARTESIAN_POINT('Ctrl Pts',(12.9031224463839,10.7132315216404,-4.85659852260819));
#19386=CARTESIAN_POINT('Ctrl Pts',(13.1606459493128,10.8908179614475,-5.03344645594301));
#19387=CARTESIAN_POINT('Ctrl Pts',(13.420203670549,11.0690158561354,-5.21120255608668));
#19388=CARTESIAN_POINT('Ctrl Pts',(13.6810302954762,11.2473763358668,-5.38931783262601));
#19389=CARTESIAN_POINT('Ctrl Pts',(13.9372302778023,11.4225729890751,-5.56427363215042));
#19390=CARTESIAN_POINT('Ctrl Pts',(14.1946545464806,11.597926588913,-5.73957562566718));
#19391=CARTESIAN_POINT('Ctrl Pts',(14.4525777950785,11.7730460975266,-5.91473898239817));
#19392=CARTESIAN_POINT('Ctrl Pts',(14.7061840816198,11.9452345625907,-6.08697056167663));
#19393=CARTESIAN_POINT('Ctrl Pts',(14.9602727846218,12.1171968581013,-6.25906787671161));
#19394=CARTESIAN_POINT('Ctrl Pts',(15.2141544107006,12.288593051788,-6.43060890607443));
#19395=CARTESIAN_POINT('Ctrl Pts',(15.4096640347459,12.4205821441381,-6.56270953374516));
#19396=CARTESIAN_POINT('Ctrl Pts',(15.6050508567907,12.5522361783515,-6.69448102850577));
#19397=CARTESIAN_POINT('Ctrl Pts',(15.8,12.6834121741351,-6.82574786431123));
#19398=CARTESIAN_POINT('Origin',(15.8,13.8493757942074,-5.91473145421246));
#19399=CARTESIAN_POINT('Origin',(15.8,0.,0.));
#19400=CARTESIAN_POINT('Origin',(13.3251262658471,0.,0.));
#19401=CARTESIAN_POINT('',(15.8,-14.4034641071566,-1.76391562154631E-15));
#19402=CARTESIAN_POINT('',(13.3251262658471,-12.1473403730037,-1.48762015059523E-15));
#19403=CARTESIAN_POINT('Origin',(15.8,0.,0.));
#19404=CARTESIAN_POINT('',(15.8,-14.2731699260464,-1.93297660315714));
#19405=CARTESIAN_POINT('Ctrl Pts',(10.0502525316942,-8.7276078365385,-2.78743136471945));
#19406=CARTESIAN_POINT('Ctrl Pts',(10.264173513818,-8.94196230434565,-2.75725731809585));
#19407=CARTESIAN_POINT('Ctrl Pts',(10.4806406238999,-9.15758913317086,-2.72628853993994));
#19408=CARTESIAN_POINT('Ctrl Pts',(10.698673871089,-9.37356359805418,-2.69475079541967));
#19409=CARTESIAN_POINT('Ctrl Pts',(10.8990914864417,-9.57208876697697,-2.66576109026303));
#19410=CARTESIAN_POINT('Ctrl Pts',(11.1008323950981,-9.77090736500581,-2.63629114159475));
#19411=CARTESIAN_POINT('Ctrl Pts',(11.3031354623541,-9.96934472627367,-2.60652505174282));
#19412=CARTESIAN_POINT('Ctrl Pts',(11.4996395060418,-10.1620938745527,-2.57761220776072));
#19413=CARTESIAN_POINT('Ctrl Pts',(11.6966739416593,-10.3544829963081,-2.54842037280583));
#19414=CARTESIAN_POINT('Ctrl Pts',(11.8935412300419,-10.5459415641124,-2.5191204383414));
#19415=CARTESIAN_POINT('Ctrl Pts',(12.0851664387448,-10.7323020728332,-2.49060068728038));
#19416=CARTESIAN_POINT('Ctrl Pts',(12.2766332831207,-10.917780824147,-2.4619788790975));
#19417=CARTESIAN_POINT('Ctrl Pts',(12.4672984745904,-11.1019006568504,-2.43340900722588));
#19418=CARTESIAN_POINT('Ctrl Pts',(12.6131381170064,-11.2427337599258,-2.41155593658665));
#19419=CARTESIAN_POINT('Ctrl Pts',(12.7585087357906,-11.3827727814342,-2.38973321279001));
#19420=CARTESIAN_POINT('Ctrl Pts',(12.9031224463839,-11.5218245801365,-2.36800640134832));
#19421=CARTESIAN_POINT('Ctrl Pts',(13.1606049656126,-11.7694041995674,-2.3293221429757));
#19422=CARTESIAN_POINT('Ctrl Pts',(13.4201210557269,-12.0180119304344,-2.29026279587101));
#19423=CARTESIAN_POINT('Ctrl Pts',(13.6809057674413,-12.2669622736816,-2.25100860979293));
#19424=CARTESIAN_POINT('Ctrl Pts',(13.9370407316157,-12.5114738741878,-2.21245431924917));
#19425=CARTESIAN_POINT('Ctrl Pts',(14.1943994820694,-12.7563158348609,-2.17371241026527));
#19426=CARTESIAN_POINT('Ctrl Pts',(14.452257261065,-13.0008872910739,-2.13494510077695));
#19427=CARTESIAN_POINT('Ctrl Pts',(14.7057618952069,-13.2413299016104,-2.09683225947821));
#19428=CARTESIAN_POINT('Ctrl Pts',(14.959748850954,-13.4815110518464,-2.0586951448823));
#19429=CARTESIAN_POINT('Ctrl Pts',(15.2135294603815,-13.7209083223233,-2.02067503134479));
#19430=CARTESIAN_POINT('Ctrl Pts',(15.409247662674,-13.9055339464685,-1.99135353081995));
#19431=CARTESIAN_POINT('Ctrl Pts',(15.6048431373525,-14.0896943197621,-1.96210138794136));
#19432=CARTESIAN_POINT('Ctrl Pts',(15.8,-14.2731699260464,-1.93297660315714));
#19433=CARTESIAN_POINT('Origin',(15.8,0.,0.));
#19434=CARTESIAN_POINT('',(15.8,-12.9772686462497,-6.24902206502841));
#19435=CARTESIAN_POINT('Ctrl Pts',(10.0502525316942,-7.43908464225652,-5.34798390487229));
#19436=CARTESIAN_POINT('Ctrl Pts',(10.2641844717857,-7.65228306925312,-5.38552777764328));
#19437=CARTESIAN_POINT('Ctrl Pts',(10.4806628006896,-7.86693728638341,-5.42270898514184));
#19438=CARTESIAN_POINT('Ctrl Pts',(10.698707376949,-8.08209794888593,-5.45945645263813));
#19439=CARTESIAN_POINT('Ctrl Pts',(10.8991296001348,-8.27986933609797,-5.49323399142585));
#19440=CARTESIAN_POINT('Ctrl Pts',(11.1008751331079,-8.47806817158807,-5.52664544938455));
#19441=CARTESIAN_POINT('Ctrl Pts',(11.3031827903456,-8.67599588377849,-5.55965742743711));
#19442=CARTESIAN_POINT('Ctrl Pts',(11.4996891833036,-8.86824792860982,-5.59172277197272));
#19443=CARTESIAN_POINT('Ctrl Pts',(11.6967259244118,-9.06024373107554,-5.62341151149102));
#19444=CARTESIAN_POINT('Ctrl Pts',(11.8935954503941,-9.25138786392987,-5.6547098697144));
#19445=CARTESIAN_POINT('Ctrl Pts',(12.0852214237498,-9.43744093804922,-5.68517460684961));
#19446=CARTESIAN_POINT('Ctrl Pts',(12.2766889707919,-9.62268689886093,-5.71526979467393));
#19447=CARTESIAN_POINT('Ctrl Pts',(12.4673547949393,-9.80662434960534,-5.74499444015009));
#19448=CARTESIAN_POINT('Ctrl Pts',(12.6131755431569,-9.94729925457443,-5.76772777509996));
#19449=CARTESIAN_POINT('Ctrl Pts',(12.7585273514378,-10.0872097382665,-5.79024463999435));
#19450=CARTESIAN_POINT('Ctrl Pts',(12.9031224463839,-10.2261519303672,-5.8125477073404));
#19451=CARTESIAN_POINT('Ctrl Pts',(13.1606063925815,-10.4735696171757,-5.85226331314787));
#19452=CARTESIAN_POINT('Ctrl Pts',(13.4201239322048,-10.7220810242639,-5.89193988397439));
#19453=CARTESIAN_POINT('Ctrl Pts',(13.6809101032503,-10.9709784873109,-5.93153701929334));
#19454=CARTESIAN_POINT('Ctrl Pts',(13.9370453939768,-11.2154370941575,-5.97042797630306));
#19455=CARTESIAN_POINT('Ctrl Pts',(14.1944044698815,-11.4602678697434,-6.00924257976788));
#19456=CARTESIAN_POINT('Ctrl Pts',(14.4522625705723,-11.7048492224773,-6.04794943640073));
#19457=CARTESIAN_POINT('Ctrl Pts',(14.7057648093973,-11.9452989904962,-6.0860024383736));
#19458=CARTESIAN_POINT('Ctrl Pts',(14.9597493558793,-12.1855075942054,-6.12395156273417));
#19459=CARTESIAN_POINT('Ctrl Pts',(15.2135275616695,-12.4249345376281,-6.161769739539));
#19460=CARTESIAN_POINT('Ctrl Pts',(15.4092463976598,-12.6095853925961,-6.19093587506459));
#19461=CARTESIAN_POINT('Ctrl Pts',(15.6048425062638,-12.7937723284765,-6.22002420721651));
#19462=CARTESIAN_POINT('Ctrl Pts',(15.8,-12.9772686462497,-6.24902206502841));
#19463=CARTESIAN_POINT('Origin',(15.8,0.,0.));
#19464=CARTESIAN_POINT('',(15.8,-10.4110618934108,-9.95336970767779));
#19465=CARTESIAN_POINT('Ctrl Pts',(10.0502525316942,-5.42237201204004,-7.38503851882133));
#19466=CARTESIAN_POINT('Ctrl Pts',(10.2643288579052,-5.61366308893708,-7.48669536435437));
#19467=CARTESIAN_POINT('Ctrl Pts',(10.4809550112864,-5.80645273316172,-7.58845719931412));
#19468=CARTESIAN_POINT('Ctrl Pts',(10.6991488645012,-5.99985821934016,-7.68996252980186));
#19469=CARTESIAN_POINT('Ctrl Pts',(10.8995930832247,-6.17753055521342,-7.78321060423707));
#19470=CARTESIAN_POINT('Ctrl Pts',(11.1013603175266,-6.35572208965081,-7.87624242157236));
#19471=CARTESIAN_POINT('Ctrl Pts',(11.3036891533892,-6.53377864760382,-7.96881028742162));
#19472=CARTESIAN_POINT('Ctrl Pts',(11.5002079767431,-6.70672218830172,-8.05872000295732));
#19473=CARTESIAN_POINT('Ctrl Pts',(11.6972566111945,-6.87953788100752,-8.14819216766752));
#19474=CARTESIAN_POINT('Ctrl Pts',(11.8941373707806,-7.05166367276733,-8.23702964306178));
#19475=CARTESIAN_POINT('Ctrl Pts',(12.0857696450343,-7.21920090191052,-8.3234988718709));
#19476=CARTESIAN_POINT('Ctrl Pts',(12.2772428756022,-7.38608422872214,-8.40936703342021));
#19477=CARTESIAN_POINT('Ctrl Pts',(12.4679136994295,-7.55183711206722,-8.49447822756625));
#19478=CARTESIAN_POINT('Ctrl Pts',(12.6135469482004,-7.67843818511105,-8.55948565482468));
#19479=CARTESIAN_POINT('Ctrl Pts',(12.7587120877915,-7.80438059757197,-8.62405202694648));
#19480=CARTESIAN_POINT('Ctrl Pts',(12.9031224463839,-7.92947038823661,-8.6881171163106));
#19481=CARTESIAN_POINT('Ctrl Pts',(13.1606452635188,-8.15253939520241,-8.80236253785699));
#19482=CARTESIAN_POINT('Ctrl Pts',(13.4202022881267,-8.3766610601629,-8.91690884941369));
#19483=CARTESIAN_POINT('Ctrl Pts',(13.6810282117054,-8.60117456124536,-9.0314987989449));
#19484=CARTESIAN_POINT('Ctrl Pts',(13.937228015869,-8.82170599546866,-9.14405633243777));
#19485=CARTESIAN_POINT('Ctrl Pts',(14.1946521067119,-9.04261517808339,-9.25665615329598));
#19486=CARTESIAN_POINT('Ctrl Pts',(14.4525751792582,-9.26332017445258,-9.36907618196659));
#19487=CARTESIAN_POINT('Ctrl Pts',(14.7061825726142,-9.48033224040404,-9.47961515062375));
#19488=CARTESIAN_POINT('Ctrl Pts',(14.9602723890249,-9.69714672451326,-9.58998050800325));
#19489=CARTESIAN_POINT('Ctrl Pts',(15.214155126052,-9.91325721198007,-9.69997936662343));
#19490=CARTESIAN_POINT('Ctrl Pts',(15.4096645113473,-10.0796790374861,-9.78468701348377));
#19491=CARTESIAN_POINT('Ctrl Pts',(15.6050510945576,-10.245684303594,-9.86917770785167));
#19492=CARTESIAN_POINT('Ctrl Pts',(15.8,-10.4110618934108,-9.95336970767779));
#19493=CARTESIAN_POINT('Origin',(15.8,0.,0.));
#19494=CARTESIAN_POINT('',(15.8,-6.82574786431122,-12.6834121741351));
#19495=CARTESIAN_POINT('Ctrl Pts',(10.0502525316942,-2.87487982939776,-8.69919410795919));
#19496=CARTESIAN_POINT('Ctrl Pts',(10.2643339107008,-3.0253983142958,-8.8549913841243));
#19497=CARTESIAN_POINT('Ctrl Pts',(10.480965237245,-3.1773096252034,-9.01135162140524));
#19498=CARTESIAN_POINT('Ctrl Pts',(10.6991643144458,-3.32988591467752,-9.16765819773448));
#19499=CARTESIAN_POINT('Ctrl Pts',(10.8996105956425,-3.47004851397084,-9.31124758570858));
#19500=CARTESIAN_POINT('Ctrl Pts',(11.1013798991834,-3.61077172321258,-9.45479172976655));
#19501=CARTESIAN_POINT('Ctrl Pts',(11.3037107883216,-3.7515099159797,-9.59785289528462));
#19502=CARTESIAN_POINT('Ctrl Pts',(11.5002306637614,-3.88820605876857,-9.73680529423691));
#19503=CARTESIAN_POINT('Ctrl Pts',(11.6972803301588,-4.0249158069733,-9.87530203177688));
#19504=CARTESIAN_POINT('Ctrl Pts',(11.8941620907594,-4.16116553050589,-10.0129819298199));
#19505=CARTESIAN_POINT('Ctrl Pts',(12.0857947176337,-4.29378265233467,-10.1469910957744));
#19506=CARTESIAN_POINT('Ctrl Pts',(12.2772682725499,-4.42596360023219,-10.2802265291355));
#19507=CARTESIAN_POINT('Ctrl Pts',(12.4679393887642,-4.5573033309954,-10.4123927004737));
#19508=CARTESIAN_POINT('Ctrl Pts',(12.6135640193753,-4.65761375114032,-10.513334312725));
#19509=CARTESIAN_POINT('Ctrl Pts',(12.7587205789998,-4.75743409091118,-10.6136529851628));
#19510=CARTESIAN_POINT('Ctrl Pts',(12.9031224463839,-4.85659852260819,-10.7132315216404));
#19511=CARTESIAN_POINT('Ctrl Pts',(13.1606459493135,-5.03344645594353,-10.890817961448));
#19512=CARTESIAN_POINT('Ctrl Pts',(13.4202036705505,-5.21120255608771,-11.0690158561365));
#19513=CARTESIAN_POINT('Ctrl Pts',(13.6810302954785,-5.38931783262757,-11.2473763358684));
#19514=CARTESIAN_POINT('Ctrl Pts',(13.9372302778055,-5.56427363215257,-11.4225729890772));
#19515=CARTESIAN_POINT('Ctrl Pts',(14.1946545464847,-5.73957562566993,-11.5979265889158));
#19516=CARTESIAN_POINT('Ctrl Pts',(14.4525777950835,-5.91473898240153,-11.77304609753));
#19517=CARTESIAN_POINT('Ctrl Pts',(14.7061840816238,-6.08697056167934,-11.9452345625935));
#19518=CARTESIAN_POINT('Ctrl Pts',(14.9602727846248,-6.25906787671367,-12.1171968581034));
#19519=CARTESIAN_POINT('Ctrl Pts',(15.2141544107027,-6.43060890607586,-12.2885930517895));
#19520=CARTESIAN_POINT('Ctrl Pts',(15.4096640347473,-6.5627095337461,-12.420582144139));
#19521=CARTESIAN_POINT('Ctrl Pts',(15.6050508567914,-6.69448102850624,-12.5522361783519));
#19522=CARTESIAN_POINT('Ctrl Pts',(15.8,-6.82574786431122,-12.6834121741351));
#19523=CARTESIAN_POINT('Origin',(15.8,0.,0.));
#19524=CARTESIAN_POINT('',(15.8,-2.57228207647107,-14.1719138864591));
#19525=CARTESIAN_POINT('Ctrl Pts',(10.0502525316942,-0.0459743785884374,
-9.16181196696065));
#19526=CARTESIAN_POINT('Ctrl Pts',(10.264326876663,-0.140978836812287,-9.35649035475255));
#19527=CARTESIAN_POINT('Ctrl Pts',(10.4809510016056,-0.237133935918953,
-9.5521345005741));
#19528=CARTESIAN_POINT('Ctrl Pts',(10.6991428064537,-0.333938024044761,
-9.74793311715205));
#19529=CARTESIAN_POINT('Ctrl Pts',(10.8995862170308,-0.422867769115888,
-9.92780487044956));
#19530=CARTESIAN_POINT('Ctrl Pts',(11.1013526405408,-0.512344667508658,
-10.1078068504782));
#19531=CARTESIAN_POINT('Ctrl Pts',(11.3036806718717,-0.601985074146152,
-10.2873541596189));
#19532=CARTESIAN_POINT('Ctrl Pts',(11.5001990829626,-0.68905155804391,-10.4617459711532));
#19533=CARTESIAN_POINT('Ctrl Pts',(11.6972473130473,-0.776271799836001,
-10.6357086581847));
#19534=CARTESIAN_POINT('Ctrl Pts',(11.8941276803915,-0.863306965607525,
-10.8087523681166));
#19535=CARTESIAN_POINT('Ctrl Pts',(12.085759816357,-0.948022038755198,-10.9771832594084));
#19536=CARTESIAN_POINT('Ctrl Pts',(12.2772329197195,-1.03256139616049,-11.1447435310826));
#19537=CARTESIAN_POINT('Ctrl Pts',(12.4679036288711,-1.11663114425741,-11.3110269536994));
#19538=CARTESIAN_POINT('Ctrl Pts',(12.6135402560747,-1.18084464940027,-11.4380362722128));
#19539=CARTESIAN_POINT('Ctrl Pts',(12.7587087591266,-1.24478452215388,-11.5643015880921));
#19540=CARTESIAN_POINT('Ctrl Pts',(12.9031224463839,-1.30832923723674,-11.6896601572689));
#19541=CARTESIAN_POINT('Ctrl Pts',(13.1606449942899,-1.42164395999531,-11.9132030828002));
#19542=CARTESIAN_POINT('Ctrl Pts',(13.4202017454155,-1.53563343890944,-12.1376081682871));
#19543=CARTESIAN_POINT('Ctrl Pts',(13.6810273936587,-1.64991426889728,-12.362278873202));
#19544=CARTESIAN_POINT('Ctrl Pts',(13.9372271276778,-1.7621682532871,-12.5829648955651));
#19545=CARTESIAN_POINT('Ctrl Pts',(14.1946511485027,-1.87470298591064,-12.8039071645252));
#19546=CARTESIAN_POINT('Ctrl Pts',(14.4525741517311,-1.98717820849243,-13.0245839618714));
#19547=CARTESIAN_POINT('Ctrl Pts',(14.706181979136,-2.09777166653541,-13.2415687303223));
#19548=CARTESIAN_POINT('Ctrl Pts',(14.9602722321832,-2.208307324337,-13.4582969085261));
#19549=CARTESIAN_POINT('Ctrl Pts',(15.2141554048834,-2.31848885998534,-13.6743147818034));
#19550=CARTESIAN_POINT('Ctrl Pts',(15.4096646971182,-2.40333699632634,-13.8406649225605));
#19551=CARTESIAN_POINT('Ctrl Pts',(15.605051187235,-2.48797565175804,-14.006594698047));
#19552=CARTESIAN_POINT('Ctrl Pts',(15.8,-2.57228207647107,-14.1719138864591));
#19553=CARTESIAN_POINT('Origin',(15.8,0.,0.));
#19554=CARTESIAN_POINT('',(15.8,1.93297660315714,-14.2731699260464));
#19555=CARTESIAN_POINT('Ctrl Pts',(10.0502525316942,2.78743136471945,-8.7276078365385));
#19556=CARTESIAN_POINT('Ctrl Pts',(10.2641735138176,2.75725731809591,-8.94196230434529));
#19557=CARTESIAN_POINT('Ctrl Pts',(10.4806406238992,2.72628853994005,-9.15758913317012));
#19558=CARTESIAN_POINT('Ctrl Pts',(10.6986738710879,2.69475079541983,-9.37356359805307));
#19559=CARTESIAN_POINT('Ctrl Pts',(10.8990914864407,2.66576109026318,-9.57208876697593));
#19560=CARTESIAN_POINT('Ctrl Pts',(11.1008323950971,2.6362911415949,-9.77090736500485));
#19561=CARTESIAN_POINT('Ctrl Pts',(11.3031354623532,2.60652505174295,-9.96934472627279));
#19562=CARTESIAN_POINT('Ctrl Pts',(11.4996395060404,2.57761220776094,-10.1620938745513));
#19563=CARTESIAN_POINT('Ctrl Pts',(11.6966739416573,2.54842037280613,-10.3544829963061));
#19564=CARTESIAN_POINT('Ctrl Pts',(11.8935412300393,2.51912043834178,-10.5459415641099));
#19565=CARTESIAN_POINT('Ctrl Pts',(12.0851664387422,2.49060068728077,-10.7323020728307));
#19566=CARTESIAN_POINT('Ctrl Pts',(12.2766332831182,2.46197887909788,-10.9177808241445));
#19567=CARTESIAN_POINT('Ctrl Pts',(12.4672984745878,2.43340900722626,-11.1019006568479));
#19568=CARTESIAN_POINT('Ctrl Pts',(12.6131381170047,2.41155593658691,-11.2427337599242));
#19569=CARTESIAN_POINT('Ctrl Pts',(12.7585087357897,2.38973321279013,-11.3827727814334));
#19570=CARTESIAN_POINT('Ctrl Pts',(12.9031224463839,2.36800640134832,-11.5218245801365));
#19571=CARTESIAN_POINT('Ctrl Pts',(13.1606049656123,2.32932214297574,-11.7694041995672));
#19572=CARTESIAN_POINT('Ctrl Pts',(13.4201210557264,2.29026279587107,-12.0180119304339));
#19573=CARTESIAN_POINT('Ctrl Pts',(13.6809057674406,2.25100860979303,-12.2669622736809));
#19574=CARTESIAN_POINT('Ctrl Pts',(13.9370407316146,2.21245431924935,-12.5114738741867));
#19575=CARTESIAN_POINT('Ctrl Pts',(14.1943994820677,2.17371241026553,-12.7563158348593));
#19576=CARTESIAN_POINT('Ctrl Pts',(14.4522572610628,2.13494510077728,-13.0008872910718));
#19577=CARTESIAN_POINT('Ctrl Pts',(14.7057618952057,2.09683225947839,-13.2413299016093));
#19578=CARTESIAN_POINT('Ctrl Pts',(14.9597488509538,2.05869514488233,-13.4815110518462));
#19579=CARTESIAN_POINT('Ctrl Pts',(15.2135294603822,2.02067503134467,-13.720908322324));
#19580=CARTESIAN_POINT('Ctrl Pts',(15.4092476626745,1.99135353081987,-13.905533946469));
#19581=CARTESIAN_POINT('Ctrl Pts',(15.6048431373528,1.96210138794132,-14.0896943197624));
#19582=CARTESIAN_POINT('Ctrl Pts',(15.8,1.93297660315714,-14.2731699260464));
#19583=CARTESIAN_POINT('Origin',(15.8,0.,0.));
#19584=CARTESIAN_POINT('',(15.8,6.24902206502841,-12.9772686462497));
#19585=CARTESIAN_POINT('Ctrl Pts',(10.0502525316942,5.34798390487229,-7.43908464225652));
#19586=CARTESIAN_POINT('Ctrl Pts',(10.2641844717853,5.3855277776432,-7.65228306925269));
#19587=CARTESIAN_POINT('Ctrl Pts',(10.4806628006887,5.42270898514168,-7.86693728638252));
#19588=CARTESIAN_POINT('Ctrl Pts',(10.6987073769477,5.4594564526379,-8.0820979488846));
#19589=CARTESIAN_POINT('Ctrl Pts',(10.8991296001334,5.49323399142562,-8.27986933609663));
#19590=CARTESIAN_POINT('Ctrl Pts',(11.1008751331065,5.52664544938432,-8.47806817158671));
#19591=CARTESIAN_POINT('Ctrl Pts',(11.3031827903442,5.55965742743688,-8.67599588377713));
#19592=CARTESIAN_POINT('Ctrl Pts',(11.4996891833017,5.59172277197241,-8.86824792860798));
#19593=CARTESIAN_POINT('Ctrl Pts',(11.6967259244095,5.62341151149064,-9.06024373107324));
#19594=CARTESIAN_POINT('Ctrl Pts',(11.8935954503913,5.65470986971394,-9.25138786392711));
#19595=CARTESIAN_POINT('Ctrl Pts',(12.085221423747,5.68517460684917,-9.43744093804651));
#19596=CARTESIAN_POINT('Ctrl Pts',(12.2766889707892,5.7152697946735,-9.62268689885829));
#19597=CARTESIAN_POINT('Ctrl Pts',(12.4673547949366,5.74499444014967,-9.80662434960277));
#19598=CARTESIAN_POINT('Ctrl Pts',(12.6131755431551,5.76772777509968,-9.94729925457273));
#19599=CARTESIAN_POINT('Ctrl Pts',(12.758527351437,5.79024463999421,-10.0872097382657));
#19600=CARTESIAN_POINT('Ctrl Pts',(12.9031224463839,5.8125477073404,-10.2261519303672));
#19601=CARTESIAN_POINT('Ctrl Pts',(13.1606063925803,5.85226331314768,-10.4735696171746));
#19602=CARTESIAN_POINT('Ctrl Pts',(13.4201239322024,5.89193988397403,-10.7220810242616));
#19603=CARTESIAN_POINT('Ctrl Pts',(13.6809101032468,5.9315370192928,-10.9709784873075));
#19604=CARTESIAN_POINT('Ctrl Pts',(13.9370453939728,5.97042797630244,-11.2154370941536));
#19605=CARTESIAN_POINT('Ctrl Pts',(14.1944044698769,6.00924257976718,-11.460267869739));
#19606=CARTESIAN_POINT('Ctrl Pts',(14.4522625705671,6.04794943639995,-11.7048492224724));
#19607=CARTESIAN_POINT('Ctrl Pts',(14.7057648093914,6.08600243837271,-11.9452989904906));
#19608=CARTESIAN_POINT('Ctrl Pts',(14.9597493558726,6.12395156273317,-12.1855075941991));
#19609=CARTESIAN_POINT('Ctrl Pts',(15.2135275616621,6.1617697395379,-12.4249345376211));
#19610=CARTESIAN_POINT('Ctrl Pts',(15.4092463976549,6.19093587506385,-12.6095853925914));
#19611=CARTESIAN_POINT('Ctrl Pts',(15.6048425062613,6.22002420721614,-12.7937723284742));
#19612=CARTESIAN_POINT('Ctrl Pts',(15.8,6.24902206502841,-12.9772686462497));
#19613=CARTESIAN_POINT('Origin',(15.8,0.,0.));
#19614=CARTESIAN_POINT('',(15.8,9.95336970767779,-10.4110618934108));
#19615=CARTESIAN_POINT('Ctrl Pts',(10.0502525316942,7.38503851882133,-5.42237201204004));
#19616=CARTESIAN_POINT('Ctrl Pts',(10.264328857905,7.48669536435428,-5.6136630889369));
#19617=CARTESIAN_POINT('Ctrl Pts',(10.480955011286,7.58845719931394,-5.80645273316137));
#19618=CARTESIAN_POINT('Ctrl Pts',(10.6991488645006,7.68996252980158,-5.99985821933963));
#19619=CARTESIAN_POINT('Ctrl Pts',(10.899593083224,7.78321060423679,-6.17753055521289));
#19620=CARTESIAN_POINT('Ctrl Pts',(11.101360317526,7.87624242157207,-6.35572208965026));
#19621=CARTESIAN_POINT('Ctrl Pts',(11.3036891533886,7.96881028742134,-6.53377864760327));
#19622=CARTESIAN_POINT('Ctrl Pts',(11.500207976743,8.05872000295729,-6.70672218830166));
#19623=CARTESIAN_POINT('Ctrl Pts',(11.697256611195,8.14819216766774,-6.87953788100794));
#19624=CARTESIAN_POINT('Ctrl Pts',(11.8941373707816,8.23702964306225,-7.05166367276824));
#19625=CARTESIAN_POINT('Ctrl Pts',(12.0857696450356,8.32349887187146,-7.21920090191162));
#19626=CARTESIAN_POINT('Ctrl Pts',(12.2772428756036,8.40936703342087,-7.38608422872343));
#19627=CARTESIAN_POINT('Ctrl Pts',(12.4679136994312,8.494478227567,-7.55183711206869));
#19628=CARTESIAN_POINT('Ctrl Pts',(12.6135469482015,8.55948565482517,-7.67843818511202));
#19629=CARTESIAN_POINT('Ctrl Pts',(12.7587120877921,8.62405202694672,-7.80438059757245));
#19630=CARTESIAN_POINT('Ctrl Pts',(12.9031224463839,8.6881171163106,-7.92947038823661));
#19631=CARTESIAN_POINT('Ctrl Pts',(13.1606452635172,8.80236253785629,-8.15253939520104));
#19632=CARTESIAN_POINT('Ctrl Pts',(13.4202022881236,8.9169088494123,-8.37666106016016));
#19633=CARTESIAN_POINT('Ctrl Pts',(13.6810282117006,9.0314987989428,-8.60117456124125));
#19634=CARTESIAN_POINT('Ctrl Pts',(13.9372280158639,9.14405633243554,-8.82170599546428));
#19635=CARTESIAN_POINT('Ctrl Pts',(14.1946521067064,9.2566561532936,-9.04261517807873));
#19636=CARTESIAN_POINT('Ctrl Pts',(14.4525751792524,9.36907618196407,-9.26332017444764));
#19637=CARTESIAN_POINT('Ctrl Pts',(14.7061825726071,9.47961515062067,-9.480332240398));
#19638=CARTESIAN_POINT('Ctrl Pts',(14.9602723890165,9.58998050799961,-9.69714672450612));
#19639=CARTESIAN_POINT('Ctrl Pts',(15.2141551260423,9.69997936661923,-9.91325721197182));
#19640=CARTESIAN_POINT('Ctrl Pts',(15.4096645113409,9.78468701348098,-10.0796790374807));
#19641=CARTESIAN_POINT('Ctrl Pts',(15.6050510945544,9.86917770785029,-10.2456843035913));
#19642=CARTESIAN_POINT('Ctrl Pts',(15.8,9.95336970767779,-10.4110618934108));
#19643=CARTESIAN_POINT('Origin',(15.8,0.,0.));
#19644=CARTESIAN_POINT('',(15.8,14.1719138864591,-2.57228207647107));
#19645=CARTESIAN_POINT('Ctrl Pts',(10.0502525316942,9.16181196696065,-0.0459743785884358));
#19646=CARTESIAN_POINT('Ctrl Pts',(10.2643268766626,9.35649035475223,-0.14097883681213));
#19647=CARTESIAN_POINT('Ctrl Pts',(10.4809510016049,9.55213450057347,-0.237133935918637));
#19648=CARTESIAN_POINT('Ctrl Pts',(10.6991428064526,9.74793311715109,-0.333938024044286));
#19649=CARTESIAN_POINT('Ctrl Pts',(10.8995862170298,9.92780487044862,-0.42286776911542));
#19650=CARTESIAN_POINT('Ctrl Pts',(11.1013526405398,10.1078068504773,-0.512344667508198));
#19651=CARTESIAN_POINT('Ctrl Pts',(11.3036806718707,10.287354159618,-0.601985074145701));
#19652=CARTESIAN_POINT('Ctrl Pts',(11.5001990829614,10.4617459711522,-0.689051558043394));
#19653=CARTESIAN_POINT('Ctrl Pts',(11.6972473130459,10.6357086581835,-0.776271799835421));
#19654=CARTESIAN_POINT('Ctrl Pts',(11.8941276803901,10.8087523681153,-0.863306965606881));
#19655=CARTESIAN_POINT('Ctrl Pts',(12.0857598163557,10.9771832594073,-0.948022038754629));
#19656=CARTESIAN_POINT('Ctrl Pts',(12.2772329197184,11.1447435310816,-1.03256139615999));
#19657=CARTESIAN_POINT('Ctrl Pts',(12.4679036288701,11.3110269536986,-1.11663114425699));
#19658=CARTESIAN_POINT('Ctrl Pts',(12.6135402560741,11.4380362722123,-1.18084464939999));
#19659=CARTESIAN_POINT('Ctrl Pts',(12.7587087591263,11.5643015880918,-1.24478452215374));
#19660=CARTESIAN_POINT('Ctrl Pts',(12.9031224463839,11.6896601572689,-1.30832923723674));
#19661=CARTESIAN_POINT('Ctrl Pts',(13.1606449942899,11.9132030828002,-1.42164395999531));
#19662=CARTESIAN_POINT('Ctrl Pts',(13.4202017454155,12.1376081682871,-1.53563343890943));
#19663=CARTESIAN_POINT('Ctrl Pts',(13.6810273936587,12.362278873202,-1.64991426889727));
#19664=CARTESIAN_POINT('Ctrl Pts',(13.9372271276793,12.5829648955663,-1.76216825328775));
#19665=CARTESIAN_POINT('Ctrl Pts',(14.1946511485057,12.8039071645278,-1.87470298591195));
#19666=CARTESIAN_POINT('Ctrl Pts',(14.4525741517356,13.0245839618753,-1.98717820849441));
#19667=CARTESIAN_POINT('Ctrl Pts',(14.7061819791402,13.2415687303259,-2.09777166653724));
#19668=CARTESIAN_POINT('Ctrl Pts',(14.9602722321871,13.4582969085294,-2.20830732433869));
#19669=CARTESIAN_POINT('Ctrl Pts',(15.214155404887,13.6743147818064,-2.31848885998689));
#19670=CARTESIAN_POINT('Ctrl Pts',(15.4096646971206,13.8406649225625,-2.40333699632737));
#19671=CARTESIAN_POINT('Ctrl Pts',(15.6050511872361,14.006594698048,-2.48797565175855));
#19672=CARTESIAN_POINT('Ctrl Pts',(15.8,14.1719138864591,-2.57228207647107));
#19673=CARTESIAN_POINT('Origin',(15.8,0.,0.));
#19674=CARTESIAN_POINT('',(15.8,14.2731699260464,1.93297660315714));
#19675=CARTESIAN_POINT('Ctrl Pts',(10.0502525316942,8.7276078365385,2.78743136471945));
#19676=CARTESIAN_POINT('Ctrl Pts',(10.2641735138176,8.94196230434521,2.75725731809592));
#19677=CARTESIAN_POINT('Ctrl Pts',(10.480640623899,9.15758913316998,2.72628853994007));
#19678=CARTESIAN_POINT('Ctrl Pts',(10.6986738710877,9.37356359805285,2.69475079541987));
#19679=CARTESIAN_POINT('Ctrl Pts',(10.8990914864403,9.57208876697557,2.66576109026324));
#19680=CARTESIAN_POINT('Ctrl Pts',(11.1008323950966,9.77090736500434,2.63629114159498));
#19681=CARTESIAN_POINT('Ctrl Pts',(11.3031354623526,9.96934472627213,2.60652505174305));
#19682=CARTESIAN_POINT('Ctrl Pts',(11.4996395060398,10.1620938745508,2.57761220776102));
#19683=CARTESIAN_POINT('Ctrl Pts',(11.6966739416569,10.3544829963057,2.54842037280618));
#19684=CARTESIAN_POINT('Ctrl Pts',(11.8935412300391,10.5459415641097,2.51912043834181));
#19685=CARTESIAN_POINT('Ctrl Pts',(12.0851664387418,10.7323020728303,2.49060068728083));
#19686=CARTESIAN_POINT('Ctrl Pts',(12.2766332831176,10.9177808241439,2.46197887909798));
#19687=CARTESIAN_POINT('Ctrl Pts',(12.467298474587,11.1019006568471,2.43340900722639));
#19688=CARTESIAN_POINT('Ctrl Pts',(12.6131381170041,11.2427337599237,2.41155593658699));
#19689=CARTESIAN_POINT('Ctrl Pts',(12.7585087357895,11.3827727814331,2.38973321279018));
#19690=CARTESIAN_POINT('Ctrl Pts',(12.9031224463839,11.5218245801365,2.36800640134832));
#19691=CARTESIAN_POINT('Ctrl Pts',(13.1606049656125,11.7694041995673,2.32932214297571));
#19692=CARTESIAN_POINT('Ctrl Pts',(13.4201210557268,12.0180119304343,2.29026279587103));
#19693=CARTESIAN_POINT('Ctrl Pts',(13.6809057674411,12.2669622736814,2.25100860979295));
#19694=CARTESIAN_POINT('Ctrl Pts',(13.9370407316154,12.5114738741875,2.21245431924923));
#19695=CARTESIAN_POINT('Ctrl Pts',(14.1943994820688,12.7563158348603,2.17371241026536));
#19696=CARTESIAN_POINT('Ctrl Pts',(14.4522572610642,13.0008872910732,2.13494510077707));
#19697=CARTESIAN_POINT('Ctrl Pts',(14.7057618952067,13.2413299016102,2.09683225947825));
#19698=CARTESIAN_POINT('Ctrl Pts',(14.9597488509542,13.4815110518466,2.05869514488227));
#19699=CARTESIAN_POINT('Ctrl Pts',(15.2135294603822,13.720908322324,2.02067503134468));
#19700=CARTESIAN_POINT('Ctrl Pts',(15.4092476626745,13.9055339464689,1.99135353081988));
#19701=CARTESIAN_POINT('Ctrl Pts',(15.6048431373528,14.0896943197624,1.96210138794133));
#19702=CARTESIAN_POINT('Ctrl Pts',(15.8,14.2731699260464,1.93297660315714));
#19703=CARTESIAN_POINT('Origin',(15.8,0.,0.));
#19704=CARTESIAN_POINT('',(15.8,12.9772686462497,6.24902206502841));
#19705=CARTESIAN_POINT('Ctrl Pts',(10.0502525316942,7.43908464225652,5.34798390487229));
#19706=CARTESIAN_POINT('Ctrl Pts',(10.2641844717852,7.65228306925265,5.3855277776432));
#19707=CARTESIAN_POINT('Ctrl Pts',(10.4806628006887,7.86693728638245,5.42270898514167));
#19708=CARTESIAN_POINT('Ctrl Pts',(10.6987073769475,8.08209794888449,5.45945645263788));
#19709=CARTESIAN_POINT('Ctrl Pts',(10.8991296001334,8.27986933609659,5.49323399142561));
#19710=CARTESIAN_POINT('Ctrl Pts',(11.1008751331065,8.47806817158674,5.52664544938433));
#19711=CARTESIAN_POINT('Ctrl Pts',(11.3031827903443,8.67599588377722,5.5596574274369));
#19712=CARTESIAN_POINT('Ctrl Pts',(11.4996891833021,8.86824792860831,5.59172277197247));
#19713=CARTESIAN_POINT('Ctrl Pts',(11.69672592441,9.06024373107381,5.62341151149074));
#19714=CARTESIAN_POINT('Ctrl Pts',(11.8935954503921,9.25138786392791,5.65470986971407));
#19715=CARTESIAN_POINT('Ctrl Pts',(12.0852214237475,9.43744093804696,5.68517460684925));
#19716=CARTESIAN_POINT('Ctrl Pts',(12.2766889707893,9.62268689885838,5.71526979467352));
#19717=CARTESIAN_POINT('Ctrl Pts',(12.4673547949364,9.80662434960252,5.74499444014963));
#19718=CARTESIAN_POINT('Ctrl Pts',(12.613175543155,9.94729925457255,5.76772777509965));
#19719=CARTESIAN_POINT('Ctrl Pts',(12.7585273514369,10.0872097382656,5.7902446399942));
#19720=CARTESIAN_POINT('Ctrl Pts',(12.9031224463839,10.2261519303672,5.8125477073404));
#19721=CARTESIAN_POINT('Ctrl Pts',(13.1606063925802,10.4735696171745,5.85226331314767));
#19722=CARTESIAN_POINT('Ctrl Pts',(13.4201239322022,10.7220810242614,5.891939883974));
#19723=CARTESIAN_POINT('Ctrl Pts',(13.6809101032465,10.9709784873072,5.93153701929276));
#19724=CARTESIAN_POINT('Ctrl Pts',(13.9370453939728,11.2154370941536,5.97042797630245));
#19725=CARTESIAN_POINT('Ctrl Pts',(14.1944044698772,11.4602678697393,6.00924257976723));
#19726=CARTESIAN_POINT('Ctrl Pts',(14.4522625705678,11.704849222473,6.04794943640006));
#19727=CARTESIAN_POINT('Ctrl Pts',(14.705764809393,11.9452989904921,6.08600243837295));
#19728=CARTESIAN_POINT('Ctrl Pts',(14.9597493558751,12.1855075942015,6.12395156273355));
#19729=CARTESIAN_POINT('Ctrl Pts',(15.2135275616656,12.4249345376244,6.16176973953841));
#19730=CARTESIAN_POINT('Ctrl Pts',(15.4092463976572,12.6095853925936,6.19093587506419));
#19731=CARTESIAN_POINT('Ctrl Pts',(15.6048425062625,12.7937723284753,6.22002420721631));
#19732=CARTESIAN_POINT('Ctrl Pts',(15.8,12.9772686462497,6.24902206502841));
#19733=CARTESIAN_POINT('Origin',(15.8,0.,0.));
#19734=CARTESIAN_POINT('',(15.8,10.4110618934108,9.9533697076778));
#19735=CARTESIAN_POINT('Ctrl Pts',(10.0502525316942,5.42237201204004,7.38503851882133));
#19736=CARTESIAN_POINT('Ctrl Pts',(10.2643288579058,5.6136630889376,7.48669536435465));
#19737=CARTESIAN_POINT('Ctrl Pts',(10.4809550112876,5.80645273316278,7.58845719931468));
#19738=CARTESIAN_POINT('Ctrl Pts',(10.699148864503,5.99985821934175,7.68996252980269));
#19739=CARTESIAN_POINT('Ctrl Pts',(10.8995930832264,6.17753055521495,7.78321060423786));
#19740=CARTESIAN_POINT('Ctrl Pts',(11.1013603175282,6.35572208965226,7.87624242157312));
#19741=CARTESIAN_POINT('Ctrl Pts',(11.3036891533908,6.5337786476052,7.96881028742234));
#19742=CARTESIAN_POINT('Ctrl Pts',(11.5002079767454,6.70672218830375,8.05872000295837));
#19743=CARTESIAN_POINT('Ctrl Pts',(11.6972566111975,6.87953788101019,8.1481921676689));
#19744=CARTESIAN_POINT('Ctrl Pts',(11.8941373707844,7.05166367277064,8.23702964306349));
#19745=CARTESIAN_POINT('Ctrl Pts',(12.0857696450381,7.21920090191376,8.32349887187257));
#19746=CARTESIAN_POINT('Ctrl Pts',(12.2772428756058,7.38608422872531,8.40936703342184));
#19747=CARTESIAN_POINT('Ctrl Pts',(12.467913699433,7.55183711207031,8.49447822756784));
#19748=CARTESIAN_POINT('Ctrl Pts',(12.6135469482027,7.6784381851131,8.55948565482573));
#19749=CARTESIAN_POINT('Ctrl Pts',(12.7587120877927,7.80438059757298,8.624052026947));
#19750=CARTESIAN_POINT('Ctrl Pts',(12.9031224463839,7.92947038823661,8.6881171163106));
#19751=CARTESIAN_POINT('Ctrl Pts',(13.1606452635176,8.15253939520139,8.80236253785647));
#19752=CARTESIAN_POINT('Ctrl Pts',(13.4202022881244,8.37666106016085,8.91690884941265));
#19753=CARTESIAN_POINT('Ctrl Pts',(13.6810282117018,8.60117456124228,9.03149879894333));
#19754=CARTESIAN_POINT('Ctrl Pts',(13.9372280158653,8.82170599546549,9.14405633243615));
#19755=CARTESIAN_POINT('Ctrl Pts',(14.1946521067081,9.04261517808011,9.25665615329431));
#19756=CARTESIAN_POINT('Ctrl Pts',(14.4525751792543,9.26332017444921,9.36907618196487));
#19757=CARTESIAN_POINT('Ctrl Pts',(14.7061825726096,9.48033224040016,9.47961515062177));
#19758=CARTESIAN_POINT('Ctrl Pts',(14.9602723890198,9.69714672450887,9.58998050800102));
#19759=CARTESIAN_POINT('Ctrl Pts',(15.2141551260462,9.91325721197517,9.69997936662094));
#19760=CARTESIAN_POINT('Ctrl Pts',(15.4096645113435,10.0796790374829,9.78468701348212));
#19761=CARTESIAN_POINT('Ctrl Pts',(15.6050510945557,10.2456843035924,9.86917770785085));
#19762=CARTESIAN_POINT('Ctrl Pts',(15.8,10.4110618934108,9.9533697076778));
#19763=CARTESIAN_POINT('Origin',(15.8,0.,0.));
#19764=CARTESIAN_POINT('',(15.8,6.82574786431122,12.6834121741351));
#19765=CARTESIAN_POINT('Ctrl Pts',(10.0502525316942,2.87487982939776,8.69919410795919));
#19766=CARTESIAN_POINT('Ctrl Pts',(10.2643339107001,3.02539831429527,8.85499138412376));
#19767=CARTESIAN_POINT('Ctrl Pts',(10.4809652372435,3.17730962520234,9.01135162140416));
#19768=CARTESIAN_POINT('Ctrl Pts',(10.6991643144436,3.32988591467592,9.16765819773286));
#19769=CARTESIAN_POINT('Ctrl Pts',(10.8996105956403,3.47004851396928,9.31124758570699));
#19770=CARTESIAN_POINT('Ctrl Pts',(11.1013798991812,3.61077172321105,9.45479172976499));
#19771=CARTESIAN_POINT('Ctrl Pts',(11.3037107883194,3.7515099159782,9.5978528952831));
#19772=CARTESIAN_POINT('Ctrl Pts',(11.5002306637591,3.88820605876695,9.73680529423527));
#19773=CARTESIAN_POINT('Ctrl Pts',(11.6972803301563,4.02491580697157,9.87530203177513));
#19774=CARTESIAN_POINT('Ctrl Pts',(11.8941620907568,4.16116553050405,10.012981929818));
#19775=CARTESIAN_POINT('Ctrl Pts',(12.085794717631,4.29378265233282,10.1469910957725));
#19776=CARTESIAN_POINT('Ctrl Pts',(12.2772682725472,4.42596360023034,10.2802265291336));
#19777=CARTESIAN_POINT('Ctrl Pts',(12.4679393887615,4.55730333099355,10.4123927004718));
#19778=CARTESIAN_POINT('Ctrl Pts',(12.6135640193735,4.6576137511391,10.5133343127237));
#19779=CARTESIAN_POINT('Ctrl Pts',(12.7587205789989,4.75743409091057,10.6136529851622));
#19780=CARTESIAN_POINT('Ctrl Pts',(12.9031224463839,4.85659852260819,10.7132315216404));
#19781=CARTESIAN_POINT('Ctrl Pts',(13.1606459493138,5.03344645594371,10.8908179614482));
#19782=CARTESIAN_POINT('Ctrl Pts',(13.4202036705511,5.21120255608808,11.0690158561368));
#19783=CARTESIAN_POINT('Ctrl Pts',(13.6810302954793,5.38931783262812,11.2473763358689));
#19784=CARTESIAN_POINT('Ctrl Pts',(13.937230277807,5.56427363215361,11.4225729890783));
#19785=CARTESIAN_POINT('Ctrl Pts',(14.1946545464869,5.73957562567147,11.5979265889173));
#19786=CARTESIAN_POINT('Ctrl Pts',(14.4525777950865,5.91473898240356,11.773046097532));
#19787=CARTESIAN_POINT('Ctrl Pts',(14.7061840816275,6.08697056168185,11.945234562596));
#19788=CARTESIAN_POINT('Ctrl Pts',(14.9602727846292,6.25906787671666,12.1171968581064));
#19789=CARTESIAN_POINT('Ctrl Pts',(15.2141544107078,6.43060890607932,12.2885930517929));
#19790=CARTESIAN_POINT('Ctrl Pts',(15.4096640347508,6.56270953374841,12.4205821441413));
#19791=CARTESIAN_POINT('Ctrl Pts',(15.6050508567931,6.69448102850738,12.5522361783531));
#19792=CARTESIAN_POINT('Ctrl Pts',(15.8,6.82574786431122,12.6834121741351));
#19793=CARTESIAN_POINT('Origin',(15.8,0.,0.));
#19794=CARTESIAN_POINT('',(15.8,2.57228207647107,14.1719138864591));
#19795=CARTESIAN_POINT('Ctrl Pts',(10.0502525316942,0.0459743785884363,
9.16181196696065));
#19796=CARTESIAN_POINT('Ctrl Pts',(10.2643268766632,0.140978836812379,9.35649035475274));
#19797=CARTESIAN_POINT('Ctrl Pts',(10.4809510016061,0.23713393591914,9.55213450057449));
#19798=CARTESIAN_POINT('Ctrl Pts',(10.6991428064543,0.333938024045044,9.74793311715262));
#19799=CARTESIAN_POINT('Ctrl Pts',(10.8995862170315,0.422867769116193,9.92780487045018));
#19800=CARTESIAN_POINT('Ctrl Pts',(11.1013526405416,0.512344667508983,10.1078068504789));
#19801=CARTESIAN_POINT('Ctrl Pts',(11.3036806718725,0.601985074146499,10.2873541596196));
#19802=CARTESIAN_POINT('Ctrl Pts',(11.5001990829629,0.689051558044051,10.4617459711535));
#19803=CARTESIAN_POINT('Ctrl Pts',(11.6972473130471,0.776271799835937,10.6357086581846));
#19804=CARTESIAN_POINT('Ctrl Pts',(11.8941276803909,0.863306965607256,10.8087523681161));
#19805=CARTESIAN_POINT('Ctrl Pts',(12.0857598163565,0.948022038754971,10.9771832594079));
#19806=CARTESIAN_POINT('Ctrl Pts',(12.2772329197191,1.0325613961603,11.1447435310822));
#19807=CARTESIAN_POINT('Ctrl Pts',(12.4679036288708,1.11663114425727,11.3110269536992));
#19808=CARTESIAN_POINT('Ctrl Pts',(12.6135402560745,1.18084464940017,11.4380362722126));
#19809=CARTESIAN_POINT('Ctrl Pts',(12.7587087591265,1.24478452215383,11.564301588092));
#19810=CARTESIAN_POINT('Ctrl Pts',(12.9031224463839,1.30832923723674,11.6896601572689));
#19811=CARTESIAN_POINT('Ctrl Pts',(13.1606449942899,1.42164395999532,11.9132030828002));
#19812=CARTESIAN_POINT('Ctrl Pts',(13.4202017454155,1.53563343890945,12.1376081682871));
#19813=CARTESIAN_POINT('Ctrl Pts',(13.6810273936588,1.64991426889729,12.362278873202));
#19814=CARTESIAN_POINT('Ctrl Pts',(13.9372271276791,1.76216825328766,12.5829648955662));
#19815=CARTESIAN_POINT('Ctrl Pts',(14.1946511485052,1.87470298591175,12.8039071645274));
#19816=CARTESIAN_POINT('Ctrl Pts',(14.4525741517349,1.9871782084941,13.0245839618747));
#19817=CARTESIAN_POINT('Ctrl Pts',(14.7061819791395,2.09777166653694,13.2415687303253));
#19818=CARTESIAN_POINT('Ctrl Pts',(14.9602722321865,2.20830732433841,13.4582969085288));
#19819=CARTESIAN_POINT('Ctrl Pts',(15.2141554048864,2.31848885998662,13.6743147818059));
#19820=CARTESIAN_POINT('Ctrl Pts',(15.4096646971202,2.40333699632719,13.8406649225621));
#19821=CARTESIAN_POINT('Ctrl Pts',(15.6050511872359,2.48797565175846,14.0065946980479));
#19822=CARTESIAN_POINT('Ctrl Pts',(15.8,2.57228207647107,14.1719138864591));
#19823=CARTESIAN_POINT('Origin',(15.8,0.,0.));
#19824=CARTESIAN_POINT('',(15.8,-1.93297660315714,14.2731699260464));
#19825=CARTESIAN_POINT('Ctrl Pts',(10.0502525316942,-2.78743136471945,8.7276078365385));
#19826=CARTESIAN_POINT('Ctrl Pts',(10.2641735138177,-2.75725731809589,8.94196230434538));
#19827=CARTESIAN_POINT('Ctrl Pts',(10.4806406238994,-2.72628853994002,9.15758913317033));
#19828=CARTESIAN_POINT('Ctrl Pts',(10.6986738710882,-2.69475079541979,9.37356359805338));
#19829=CARTESIAN_POINT('Ctrl Pts',(10.899091486441,-2.66576109026313,9.57208876697628));
#19830=CARTESIAN_POINT('Ctrl Pts',(11.1008323950975,-2.63629114159484,9.77090736500523));
#19831=CARTESIAN_POINT('Ctrl Pts',(11.3031354623537,-2.60652505174289,9.9693447262732));
#19832=CARTESIAN_POINT('Ctrl Pts',(11.4996395060412,-2.57761220776082,10.1620938745521));
#19833=CARTESIAN_POINT('Ctrl Pts',(11.6966739416585,-2.54842037280596,10.3544829963072));
#19834=CARTESIAN_POINT('Ctrl Pts',(11.8935412300409,-2.51912043834155,10.5459415641114));
#19835=CARTESIAN_POINT('Ctrl Pts',(12.0851664387437,-2.49060068728054,10.7323020728322));
#19836=CARTESIAN_POINT('Ctrl Pts',(12.2766332831197,-2.46197887909766,10.9177808241459));
#19837=CARTESIAN_POINT('Ctrl Pts',(12.4672984745893,-2.43340900722605,11.1019006568493));
#19838=CARTESIAN_POINT('Ctrl Pts',(12.6131381170056,-2.41155593658676,11.2427337599251));
#19839=CARTESIAN_POINT('Ctrl Pts',(12.7585087357902,-2.38973321279006,11.3827727814338));
#19840=CARTESIAN_POINT('Ctrl Pts',(12.9031224463839,-2.36800640134832,11.5218245801365));
#19841=CARTESIAN_POINT('Ctrl Pts',(13.1606049656133,-2.3293221429756,11.769404199568));
#19842=CARTESIAN_POINT('Ctrl Pts',(13.4201210557283,-2.2902627958708,12.0180119304357));
#19843=CARTESIAN_POINT('Ctrl Pts',(13.6809057674434,-2.25100860979261,12.2669622736836));
#19844=CARTESIAN_POINT('Ctrl Pts',(13.9370407316176,-2.21245431924889,12.5114738741896));
#19845=CARTESIAN_POINT('Ctrl Pts',(14.194399482071,-2.17371241026503,12.7563158348624));
#19846=CARTESIAN_POINT('Ctrl Pts',(14.4522572610663,-2.13494510077675,13.0008872910752));
#19847=CARTESIAN_POINT('Ctrl Pts',(14.7057618952085,-2.09683225947798,13.2413299016119));
#19848=CARTESIAN_POINT('Ctrl Pts',(14.9597488509557,-2.05869514488204,13.481511051848));
#19849=CARTESIAN_POINT('Ctrl Pts',(15.2135294603834,-2.0206750313445,13.7209083223251));
#19850=CARTESIAN_POINT('Ctrl Pts',(15.4092476626753,-1.99135353081976,13.9055339464697));
#19851=CARTESIAN_POINT('Ctrl Pts',(15.6048431373532,-1.96210138794127,14.0896943197627));
#19852=CARTESIAN_POINT('Ctrl Pts',(15.8,-1.93297660315714,14.2731699260464));
#19853=CARTESIAN_POINT('Origin',(15.8,0.,0.));
#19854=CARTESIAN_POINT('',(15.8,-6.24902206502841,12.9772686462497));
#19855=CARTESIAN_POINT('Ctrl Pts',(10.0502525316942,-5.34798390487229,7.43908464225652));
#19856=CARTESIAN_POINT('Ctrl Pts',(10.2641844717849,-5.38552777764315,7.65228306925236));
#19857=CARTESIAN_POINT('Ctrl Pts',(10.4806628006881,-5.42270898514157,7.86693728638186));
#19858=CARTESIAN_POINT('Ctrl Pts',(10.6987073769466,-5.45945645263773,8.08209794888361));
#19859=CARTESIAN_POINT('Ctrl Pts',(10.8991296001323,-5.49323399142543,8.27986933609552));
#19860=CARTESIAN_POINT('Ctrl Pts',(11.1008751331052,-5.52664544938412,8.47806817158548));
#19861=CARTESIAN_POINT('Ctrl Pts',(11.3031827903428,-5.55965742743666,8.67599588377579));
#19862=CARTESIAN_POINT('Ctrl Pts',(11.4996891833007,-5.59172277197224,8.86824792860694));
#19863=CARTESIAN_POINT('Ctrl Pts',(11.6967259244087,-5.62341151149052,9.0602437310725));
#19864=CARTESIAN_POINT('Ctrl Pts',(11.8935954503908,-5.65470986971387,9.25138786392667));
#19865=CARTESIAN_POINT('Ctrl Pts',(12.0852214237466,-5.68517460684912,9.43744093804618));
#19866=CARTESIAN_POINT('Ctrl Pts',(12.2766889707889,-5.71526979467347,9.62268689885806));
#19867=CARTESIAN_POINT('Ctrl Pts',(12.4673547949365,-5.74499444014965,9.80662434960265));
#19868=CARTESIAN_POINT('Ctrl Pts',(12.613175543155,-5.76772777509967,9.94729925457264));
#19869=CARTESIAN_POINT('Ctrl Pts',(12.7585273514369,-5.79024463999421,10.0872097382656));
#19870=CARTESIAN_POINT('Ctrl Pts',(12.9031224463839,-5.8125477073404,10.2261519303672));
#19871=CARTESIAN_POINT('Ctrl Pts',(13.1606063925794,-5.85226331314755,10.4735696171738));
#19872=CARTESIAN_POINT('Ctrl Pts',(13.4201239322007,-5.89193988397376,10.7220810242599));
#19873=CARTESIAN_POINT('Ctrl Pts',(13.6809101032441,-5.93153701929241,10.970978487305));
#19874=CARTESIAN_POINT('Ctrl Pts',(13.9370453939694,-5.97042797630194,11.2154370941504));
#19875=CARTESIAN_POINT('Ctrl Pts',(14.1944044698729,-6.00924257976658,11.4602678697352));
#19876=CARTESIAN_POINT('Ctrl Pts',(14.4522625705624,-6.04794943639925,11.7048492224679));
#19877=CARTESIAN_POINT('Ctrl Pts',(14.7057648093879,-6.08600243837219,11.9452989904873));
#19878=CARTESIAN_POINT('Ctrl Pts',(14.9597493558704,-6.12395156273284,12.185507594197));
#19879=CARTESIAN_POINT('Ctrl Pts',(15.213527561661,-6.16176973953774,12.4249345376201));
#19880=CARTESIAN_POINT('Ctrl Pts',(15.4092463976542,-6.19093587506375,12.6095853925908));
#19881=CARTESIAN_POINT('Ctrl Pts',(15.604842506261,-6.22002420721609,12.7937723284739));
#19882=CARTESIAN_POINT('Ctrl Pts',(15.8,-6.24902206502841,12.9772686462497));
#19883=CARTESIAN_POINT('Origin',(15.8,0.,0.));
#19884=CARTESIAN_POINT('',(15.8,-9.95336970767779,10.4110618934108));
#19885=CARTESIAN_POINT('Ctrl Pts',(10.0502525316942,-7.38503851882133,5.42237201204004));
#19886=CARTESIAN_POINT('Ctrl Pts',(10.2643288579052,-7.48669536435435,5.61366308893702));
#19887=CARTESIAN_POINT('Ctrl Pts',(10.4809550112863,-7.58845719931407,5.80645273316162));
#19888=CARTESIAN_POINT('Ctrl Pts',(10.699148864501,-7.68996252980178,5.99985821934));
#19889=CARTESIAN_POINT('Ctrl Pts',(10.8995930832245,-7.78321060423697,6.17753055521325));
#19890=CARTESIAN_POINT('Ctrl Pts',(11.1013603175263,-7.87624242157225,6.35572208965061));
#19891=CARTESIAN_POINT('Ctrl Pts',(11.3036891533889,-7.96881028742151,6.5337786476036));
#19892=CARTESIAN_POINT('Ctrl Pts',(11.5002079767434,-8.05872000295745,6.70672218830198));
#19893=CARTESIAN_POINT('Ctrl Pts',(11.6972566111953,-8.14819216766789,6.87953788100824));
#19894=CARTESIAN_POINT('Ctrl Pts',(11.8941373707819,-8.23702964306239,7.05166367276852));
#19895=CARTESIAN_POINT('Ctrl Pts',(12.0857696450361,-8.32349887187168,7.21920090191204));
#19896=CARTESIAN_POINT('Ctrl Pts',(12.2772428756043,-8.40936703342116,7.38608422872399));
#19897=CARTESIAN_POINT('Ctrl Pts',(12.467913699432,-8.49447822756735,7.55183711206938));
#19898=CARTESIAN_POINT('Ctrl Pts',(12.613546948202,-8.55948565482541,7.67843818511248));
#19899=CARTESIAN_POINT('Ctrl Pts',(12.7587120877923,-8.62405202694684,7.80438059757268));
#19900=CARTESIAN_POINT('Ctrl Pts',(12.9031224463839,-8.6881171163106,7.92947038823661));
#19901=CARTESIAN_POINT('Ctrl Pts',(13.1606452635168,-8.80236253785607,8.15253939520062));
#19902=CARTESIAN_POINT('Ctrl Pts',(13.4202022881226,-8.91690884941186,8.37666106015931));
#19903=CARTESIAN_POINT('Ctrl Pts',(13.6810282116991,-9.03149879894215,8.60117456123998));
#19904=CARTESIAN_POINT('Ctrl Pts',(13.9372280158629,-9.14405633243508,8.82170599546338));
#19905=CARTESIAN_POINT('Ctrl Pts',(14.1946521067058,-9.25665615329334,9.04261517807822));
#19906=CARTESIAN_POINT('Ctrl Pts',(14.4525751792523,-9.36907618196402,9.26332017444753));
#19907=CARTESIAN_POINT('Ctrl Pts',(14.7061825726078,-9.47961515062096,9.48033224039856));
#19908=CARTESIAN_POINT('Ctrl Pts',(14.960272389018,-9.58998050800025,9.69714672450736));
#19909=CARTESIAN_POINT('Ctrl Pts',(15.2141551260446,-9.69997936662022,9.91325721197376));
#19910=CARTESIAN_POINT('Ctrl Pts',(15.4096645113424,-9.78468701348163,10.0796790374819));
#19911=CARTESIAN_POINT('Ctrl Pts',(15.6050510945551,-9.86917770785061,10.2456843035919));
#19912=CARTESIAN_POINT('Ctrl Pts',(15.8,-9.95336970767779,10.4110618934108));
#19913=CARTESIAN_POINT('Origin',(15.8,0.,0.));
#19914=CARTESIAN_POINT('',(15.8,-12.6834121741351,6.82574786431122));
#19915=CARTESIAN_POINT('Ctrl Pts',(10.0502525316942,-8.69919410795919,2.87487982939776));
#19916=CARTESIAN_POINT('Ctrl Pts',(10.264333910701,-8.85499138412439,3.02539831429588));
#19917=CARTESIAN_POINT('Ctrl Pts',(10.4809652372453,-9.01135162140542,3.17730962520357));
#19918=CARTESIAN_POINT('Ctrl Pts',(10.6991643144462,-9.16765819773475,3.32988591467777));
#19919=CARTESIAN_POINT('Ctrl Pts',(10.8996105956429,-9.31124758570884,3.47004851397109));
#19920=CARTESIAN_POINT('Ctrl Pts',(11.1013798991838,-9.4547917297668,3.61077172321283));
#19921=CARTESIAN_POINT('Ctrl Pts',(11.3037107883219,-9.59785289528487,3.75150991597994));
#19922=CARTESIAN_POINT('Ctrl Pts',(11.5002306637619,-9.73680529423722,3.88820605876887));
#19923=CARTESIAN_POINT('Ctrl Pts',(11.6972803301593,-9.87530203177726,4.02491580697367));
#19924=CARTESIAN_POINT('Ctrl Pts',(11.8941620907601,-10.0129819298203,4.16116553050634));
#19925=CARTESIAN_POINT('Ctrl Pts',(12.0857947176342,-10.1469910957747,4.29378265233503));
#19926=CARTESIAN_POINT('Ctrl Pts',(12.2772682725503,-10.2802265291358,4.42596360023247));
#19927=CARTESIAN_POINT('Ctrl Pts',(12.4679393887645,-10.4123927004739,4.55730333099561));
#19928=CARTESIAN_POINT('Ctrl Pts',(12.6135640193755,-10.5133343127251,4.65761375114046));
#19929=CARTESIAN_POINT('Ctrl Pts',(12.7587205789999,-10.6136529851629,4.75743409091125));
#19930=CARTESIAN_POINT('Ctrl Pts',(12.9031224463839,-10.7132315216404,4.85659852260819));
#19931=CARTESIAN_POINT('Ctrl Pts',(13.1606459493129,-10.8908179614476,5.03344645594312));
#19932=CARTESIAN_POINT('Ctrl Pts',(13.4202036705494,-11.0690158561357,5.2112025560869));
#19933=CARTESIAN_POINT('Ctrl Pts',(13.6810302954767,-11.2473763358671,5.38931783262634));
#19934=CARTESIAN_POINT('Ctrl Pts',(13.9372302778033,-11.4225729890757,5.56427363215107));
#19935=CARTESIAN_POINT('Ctrl Pts',(14.1946545464821,-11.597926588914,5.73957562566816));
#19936=CARTESIAN_POINT('Ctrl Pts',(14.4525777950805,-11.7730460975279,5.91473898239949));
#19937=CARTESIAN_POINT('Ctrl Pts',(14.7061840816217,-11.9452345625921,6.08697056167794));
#19938=CARTESIAN_POINT('Ctrl Pts',(14.9602727846237,-12.1171968581026,6.25906787671289));
#19939=CARTESIAN_POINT('Ctrl Pts',(15.2141544107024,-12.2885930517893,6.43060890607568));
#19940=CARTESIAN_POINT('Ctrl Pts',(15.4096640347472,-12.4205821441389,6.562709533746));
#19941=CARTESIAN_POINT('Ctrl Pts',(15.6050508567913,-12.5522361783519,6.69448102850619));
#19942=CARTESIAN_POINT('Ctrl Pts',(15.8,-12.6834121741351,6.82574786431122));
#19943=CARTESIAN_POINT('Origin',(15.8,0.,0.));
#19944=CARTESIAN_POINT('',(15.8,-14.1719138864591,2.57228207647107));
#19945=CARTESIAN_POINT('Ctrl Pts',(10.0502525316942,-9.16181196696065,0.0459743785884369));
#19946=CARTESIAN_POINT('Ctrl Pts',(10.2643268766627,-9.35649035475233,0.14097883681218));
#19947=CARTESIAN_POINT('Ctrl Pts',(10.4809510016051,-9.55213450057367,0.237133935918737));
#19948=CARTESIAN_POINT('Ctrl Pts',(10.699142806453,-9.74793311715139,0.333938024044436));
#19949=CARTESIAN_POINT('Ctrl Pts',(10.8995862170302,-9.92780487044902,0.422867769115622));
#19950=CARTESIAN_POINT('Ctrl Pts',(11.1013526405404,-10.1078068504778,0.512344667508452));
#19951=CARTESIAN_POINT('Ctrl Pts',(11.3036806718714,-10.2873541596186,0.601985074146008));
#19952=CARTESIAN_POINT('Ctrl Pts',(11.5001990829621,-10.4617459711528,0.68905155804369));
#19953=CARTESIAN_POINT('Ctrl Pts',(11.6972473130466,-10.6357086581841,0.776271799835705));
#19954=CARTESIAN_POINT('Ctrl Pts',(11.8941276803907,-10.8087523681159,0.863306965607153));
#19955=CARTESIAN_POINT('Ctrl Pts',(12.0857598163563,-10.9771832594078,0.948022038754891));
#19956=CARTESIAN_POINT('Ctrl Pts',(12.2772329197189,-11.1447435310821,1.03256139616025));
#19957=CARTESIAN_POINT('Ctrl Pts',(12.4679036288707,-11.3110269536991,1.11663114425723));
#19958=CARTESIAN_POINT('Ctrl Pts',(12.6135402560745,-11.4380362722126,1.18084464940015));
#19959=CARTESIAN_POINT('Ctrl Pts',(12.7587087591265,-11.564301588092,1.24478452215382));
#19960=CARTESIAN_POINT('Ctrl Pts',(12.9031224463839,-11.6896601572689,1.30832923723674));
#19961=CARTESIAN_POINT('Ctrl Pts',(13.1606449942899,-11.9132030828002,1.42164395999532));
#19962=CARTESIAN_POINT('Ctrl Pts',(13.4202017454155,-12.1376081682871,1.53563343890945));
#19963=CARTESIAN_POINT('Ctrl Pts',(13.6810273936588,-12.362278873202,1.64991426889729));
#19964=CARTESIAN_POINT('Ctrl Pts',(13.9372271276793,-12.5829648955663,1.76216825328774));
#19965=CARTESIAN_POINT('Ctrl Pts',(14.1946511485056,-12.8039071645277,1.8747029859119));
#19966=CARTESIAN_POINT('Ctrl Pts',(14.4525741517354,-13.0245839618751,1.98717820849432));
#19967=CARTESIAN_POINT('Ctrl Pts',(14.70618197914,-13.2415687303257,2.09777166653716));
#19968=CARTESIAN_POINT('Ctrl Pts',(14.9602722321869,-13.4582969085292,2.20830732433861));
#19969=CARTESIAN_POINT('Ctrl Pts',(15.2141554048868,-13.6743147818063,2.31848885998681));
#19970=CARTESIAN_POINT('Ctrl Pts',(15.4096646971205,-13.8406649225624,2.40333699632732));
#19971=CARTESIAN_POINT('Ctrl Pts',(15.6050511872361,-14.006594698048,2.48797565175852));
#19972=CARTESIAN_POINT('Ctrl Pts',(15.8,-14.1719138864591,2.57228207647107));
#19973=CARTESIAN_POINT('Origin',(15.8,0.,0.));
#19974=CARTESIAN_POINT('Ctrl Pts',(10.0502525316942,9.36936257048691,-5.29266352931554));
#19975=CARTESIAN_POINT('Ctrl Pts',(11.9668350211294,10.5998888833726,-7.11242577089739));
#19976=CARTESIAN_POINT('Ctrl Pts',(13.8834175105647,11.8304151962582,-8.93218801247923));
#19977=CARTESIAN_POINT('Ctrl Pts',(15.8,13.0609415091439,-10.7519502540611));
#19978=CARTESIAN_POINT('Ctrl Pts',(10.0502525316942,9.19066745032221,-5.50090730964532));
#19979=CARTESIAN_POINT('Ctrl Pts',(11.9668350211294,10.3756997001811,-7.33966268788185));
#19980=CARTESIAN_POINT('Ctrl Pts',(13.8834175105647,11.5602999829831,-9.17890569898124));
#19981=CARTESIAN_POINT('Ctrl Pts',(15.8,12.745332232842,-11.0176610772178));
#19982=CARTESIAN_POINT('Ctrl Pts',(10.0502525316942,8.88494866314842,-5.78937538435654));
#19983=CARTESIAN_POINT('Ctrl Pts',(11.9668350211294,9.99448540715111,-7.65168842520524));
#19984=CARTESIAN_POINT('Ctrl Pts',(13.8834175105647,11.104545703274,-9.51341402508185));
#19985=CARTESIAN_POINT('Ctrl Pts',(15.8,12.2140824472767,-11.3757270659305));
#19986=CARTESIAN_POINT('Ctrl Pts',(10.0502525316942,8.62956238511758,-5.83613263565859));
#19987=CARTESIAN_POINT('Ctrl Pts',(11.9668350211294,9.68562073924798,-7.68881403767578));
#19988=CARTESIAN_POINT('Ctrl Pts',(13.8834175105647,10.7414245752752,-9.54180236671467));
#19989=CARTESIAN_POINT('Ctrl Pts',(15.8,11.7974829294057,-11.3944837687319));
#19990=CARTESIAN_POINT('Ctrl Pts',(10.0502525316942,8.45485763321061,-5.80103525788047));
#19991=CARTESIAN_POINT('Ctrl Pts',(11.9668350211294,9.47972276943763,-7.63326974588331));
#19992=CARTESIAN_POINT('Ctrl Pts',(13.8834175105647,10.5043553237743,-9.46570011434023));
#19993=CARTESIAN_POINT('Ctrl Pts',(15.8,11.5292204600013,-11.2979346023431));
#19994=CARTESIAN_POINT('Ctrl Pts',(10.0502525316941,8.27718317134364,-5.77456941285603));
#19995=CARTESIAN_POINT('Ctrl Pts',(11.9668350211294,9.27115170336996,-7.58519358293628));
#19996=CARTESIAN_POINT('Ctrl Pts',(13.8834175105647,10.2649338319875,-9.39609248134292));
#19997=CARTESIAN_POINT('Ctrl Pts',(15.8,11.2589023640139,-11.2067166514232));
#19998=CARTESIAN_POINT('Ctrl Pts',(10.0502525316942,8.0031076613001,-5.75553891274797));
#19999=CARTESIAN_POINT('Ctrl Pts',(11.9668350211295,8.94781145509674,-7.53737545292391));
#20000=CARTESIAN_POINT('Ctrl Pts',(13.8834175105647,9.89241088219743,-9.31923862861202));
#20001=CARTESIAN_POINT('Ctrl Pts',(15.8,10.8371146759941,-11.101075168788));
#20002=CARTESIAN_POINT('Ctrl Pts',(10.0502525316942,7.76245969237558,-5.66702291215723));
#20003=CARTESIAN_POINT('Ctrl Pts',(11.9668350211294,8.66825218904355,-7.4114007810768));
#20004=CARTESIAN_POINT('Ctrl Pts',(13.8834175105647,9.57397375447812,-9.15584481177961));
#20005=CARTESIAN_POINT('Ctrl Pts',(15.8,10.4797662511461,-10.9002226806992));
#20006=CARTESIAN_POINT('Ctrl Pts',(10.0502525316942,7.54398815168985,-5.55269814935976));
#20007=CARTESIAN_POINT('Ctrl Pts',(11.9668350211294,8.41867077420535,-7.25492061800101));
#20008=CARTESIAN_POINT('Ctrl Pts',(13.8834175105647,9.29328875951754,-8.95722517253277));
#20009=CARTESIAN_POINT('Ctrl Pts',(15.8,10.167971382033,-10.659447641174));
#20010=CARTESIAN_POINT('Ctrl Pts',(10.0502525316942,7.44587907063767,-5.47835809159451));
#20011=CARTESIAN_POINT('Ctrl Pts',(11.9668350211294,8.30851053998513,-7.15753678028296));
#20012=CARTESIAN_POINT('Ctrl Pts',(13.8834175105647,9.17110734047641,-8.83668456248994));
#20013=CARTESIAN_POINT('Ctrl Pts',(15.8,10.0337388098239,-10.5158632511784));
#20014=CARTESIAN_POINT('Ctrl Pts',(10.0502525316942,7.38503851882133,-5.42237201204004));
#20015=CARTESIAN_POINT('Ctrl Pts',(11.9668350211294,8.24114891510682,-7.08526863916361));
#20016=CARTESIAN_POINT('Ctrl Pts',(13.8834175105647,9.09725931139231,-8.74816526628719));
#20017=CARTESIAN_POINT('Ctrl Pts',(15.8,9.95336970767779,-10.4110618934108));
#20018=CARTESIAN_POINT('Ctrl Pts',(15.8,9.9801646912522,-10.4452137610133));
#20019=CARTESIAN_POINT('Ctrl Pts',(15.8,9.97473811086981,-10.4384530463692));
#20020=CARTESIAN_POINT('Ctrl Pts',(15.8,9.96934533045351,-10.4316574943231));
#20021=CARTESIAN_POINT('Ctrl Pts',(15.8,9.96398633981914,-10.4248271146823));
#20022=CARTESIAN_POINT('Ctrl Pts',(15.8,9.95866113228077,-10.4179619142908));
#20023=CARTESIAN_POINT('Ctrl Pts',(15.8,9.95336970767779,-10.4110618934108));
#20024=CARTESIAN_POINT('Origin',(15.8,11.3437865591856,-9.90493637355978));
#20025=CARTESIAN_POINT('Ctrl Pts',(10.0502525316942,7.27527035012649,-7.92891439885425));
#20026=CARTESIAN_POINT('Ctrl Pts',(11.9668350211294,7.88323296009842,-10.0398646795257));
#20027=CARTESIAN_POINT('Ctrl Pts',(13.8834175105647,8.49119557007034,-12.1508149601973));
#20028=CARTESIAN_POINT('Ctrl Pts',(15.8,9.09915818004226,-14.2617652408688));
#20029=CARTESIAN_POINT('Ctrl Pts',(10.0502525316942,7.04097032456894,-8.07174617417206));
#20030=CARTESIAN_POINT('Ctrl Pts',(11.9668350211294,7.59972129962697,-10.186749261509));
#20031=CARTESIAN_POINT('Ctrl Pts',(13.8834175105647,8.15813578620935,-12.3019395333854));
#20032=CARTESIAN_POINT('Ctrl Pts',(15.8,8.71688676126738,-14.4169426207224));
#20033=CARTESIAN_POINT('Ctrl Pts',(10.0502525316942,6.66138127597021,-8.25126590443755));
#20034=CARTESIAN_POINT('Ctrl Pts',(11.9668350211294,7.14127838379809,-10.365200404417));
#20035=CARTESIAN_POINT('Ctrl Pts',(13.8834175105647,7.62165928459737,-12.4788866778492));
#20036=CARTESIAN_POINT('Ctrl Pts',(15.8,8.10155639242524,-14.5928211778287));
#20037=CARTESIAN_POINT('Ctrl Pts',(10.0502525316942,6.42930419296208,-8.22079862024226));
#20038=CARTESIAN_POINT('Ctrl Pts',(11.9668350211294,6.86580395314969,-10.3118069242151));
#20039=CARTESIAN_POINT('Ctrl Pts',(13.8834175105647,7.30234839548018,-12.4027801127282));
#20040=CARTESIAN_POINT('Ctrl Pts',(15.8,7.73884815566778,-14.493788416701));
#20041=CARTESIAN_POINT('Ctrl Pts',(10.0502525316942,6.30697938690418,-8.16221173215364));
#20042=CARTESIAN_POINT('Ctrl Pts',(11.9668350211294,6.72434771418859,-10.2323186327506));
#20043=CARTESIAN_POINT('Ctrl Pts',(13.8834175105647,7.14137150628508,-12.3026176380752));
#20044=CARTESIAN_POINT('Ctrl Pts',(15.8,7.55873983356949,-14.3727245386721));
#20045=CARTESIAN_POINT('Ctrl Pts',(10.0502525316942,6.22815403351084,-8.12000643506485));
#20046=CARTESIAN_POINT('Ctrl Pts',(11.9668350211294,6.63375833246635,-10.1755454476056));
#20047=CARTESIAN_POINT('Ctrl Pts',(13.8834175105647,7.03916552489902,-12.2311493413123));
#20048=CARTESIAN_POINT('Ctrl Pts',(15.8,7.44476982385453,-14.2866883538531));
#20049=CARTESIAN_POINT('Ctrl Pts',(10.0502525316942,6.08789997184504,-8.04942040067478));
#20050=CARTESIAN_POINT('Ctrl Pts',(11.9668350211294,6.47376321403758,-10.0785454407991));
#20051=CARTESIAN_POINT('Ctrl Pts',(13.8834175105647,6.85942462405721,-12.1078515605739));
#20052=CARTESIAN_POINT('Ctrl Pts',(15.8,7.24528786624975,-14.1369766006982));
#20053=CARTESIAN_POINT('Ctrl Pts',(10.0502525316942,5.83267830770084,-7.94713925110582));
#20054=CARTESIAN_POINT('Ctrl Pts',(11.9668350211294,6.18048893841472,-9.93371906448111));
#20055=CARTESIAN_POINT('Ctrl Pts',(13.8834175105647,6.52817426230452,-11.920292369998));
#20056=CARTESIAN_POINT('Ctrl Pts',(15.8,6.8759848930184,-13.9068721833733));
#20057=CARTESIAN_POINT('Ctrl Pts',(10.0502525316942,5.63138575926581,-7.78832910259187));
#20058=CARTESIAN_POINT('Ctrl Pts',(11.9668350211294,5.95382183425817,-9.7272251121909));
#20059=CARTESIAN_POINT('Ctrl Pts',(13.8834175105647,6.27616146093386,-11.6661698490829));
#20060=CARTESIAN_POINT('Ctrl Pts',(15.8,6.59859753592622,-13.605065858682));
#20061=CARTESIAN_POINT('Ctrl Pts',(10.0502525316942,5.45884429554415,-7.61219406851115));
#20062=CARTESIAN_POINT('Ctrl Pts',(11.9668350211294,5.7646862128331,-9.50140467053762));
#20063=CARTESIAN_POINT('Ctrl Pts',(13.8834175105647,6.07045912241827,-11.3906602079427));
#20064=CARTESIAN_POINT('Ctrl Pts',(15.8,6.37630103970722,-13.2798708099692));
#20065=CARTESIAN_POINT('Ctrl Pts',(10.0502525316942,5.38854605810145,-7.51113133249701));
#20066=CARTESIAN_POINT('Ctrl Pts',(11.9668350211294,5.69007333772413,-9.37468648227302));
#20067=CARTESIAN_POINT('Ctrl Pts',(13.8834175105647,5.99154494312677,-11.238220929081));
#20068=CARTESIAN_POINT('Ctrl Pts',(15.8,6.29307222274945,-13.101776078857));
#20069=CARTESIAN_POINT('Ctrl Pts',(10.0502525316942,5.34798390487229,-7.43908464225652));
#20070=CARTESIAN_POINT('Ctrl Pts',(11.9668350211294,5.64832995825766,-9.28514597692092));
#20071=CARTESIAN_POINT('Ctrl Pts',(13.8834175105647,5.94867601164304,-11.1312073115853));
#20072=CARTESIAN_POINT('Ctrl Pts',(15.8,6.24902206502841,-12.9772686462497));
#20073=CARTESIAN_POINT('Ctrl Pts',(15.8,6.26395210128206,-13.0180291077652));
#20074=CARTESIAN_POINT('Ctrl Pts',(15.8,6.26088029236732,-13.0099223804886));
#20075=CARTESIAN_POINT('Ctrl Pts',(15.8,6.25785139447984,-13.0017929656379));
#20076=CARTESIAN_POINT('Ctrl Pts',(15.8,6.2548653949033,-12.993640869393));
#20077=CARTESIAN_POINT('Ctrl Pts',(15.8,6.25192228516408,-12.985466096197));
#20078=CARTESIAN_POINT('Ctrl Pts',(15.8,6.24902206502841,-12.9772686462497));
#20079=CARTESIAN_POINT('Origin',(15.8,7.7277884589423,-12.9255771089134));
#20080=CARTESIAN_POINT('Ctrl Pts',(10.0502525316942,4.46902397810654,-9.78902788303806));
#20081=CARTESIAN_POINT('Ctrl Pts',(11.9668350211294,4.39491126897609,-11.9845316814717));
#20082=CARTESIAN_POINT('Ctrl Pts',(13.8834175105647,4.32079855984563,-14.1800354799052));
#20083=CARTESIAN_POINT('Ctrl Pts',(15.8,4.24668585071518,-16.3755392783388));
#20084=CARTESIAN_POINT('Ctrl Pts',(10.0502525316942,4.20205396612197,-9.8524662840083));
#20085=CARTESIAN_POINT('Ctrl Pts',(11.9668350211294,4.07988582479457,-12.036617299121));
#20086=CARTESIAN_POINT('Ctrl Pts',(13.8834175105647,3.95733982070598,-14.2208423566523));
#20087=CARTESIAN_POINT('Ctrl Pts',(15.8,3.83517167937858,-16.404993371765));
#20088=CARTESIAN_POINT('Ctrl Pts',(10.0502525316942,3.7855656109216,-9.90590216992165));
#20089=CARTESIAN_POINT('Ctrl Pts',(11.9668350211295,3.58873319698334,-12.0646697130184));
#20090=CARTESIAN_POINT('Ctrl Pts',(13.8834175105647,3.39243568541408,-14.2233509855394));
#20091=CARTESIAN_POINT('Ctrl Pts',(15.8,3.19560327147581,-16.3821185286362));
#20092=CARTESIAN_POINT('Ctrl Pts',(10.0502525316942,3.57425782911966,-9.80521299123422));
#20093=CARTESIAN_POINT('Ctrl Pts',(11.9668350211295,3.34323666910061,-11.9287659082934));
#20094=CARTESIAN_POINT('Ctrl Pts',(13.8834175105647,3.11226431322855,-14.0522999619539));
#20095=CARTESIAN_POINT('Ctrl Pts',(15.8,2.8812431532095,-16.1758528790132));
#20096=CARTESIAN_POINT('Ctrl Pts',(10.0502525316942,3.47602249721152,-9.71169428155716));
#20097=CARTESIAN_POINT('Ctrl Pts',(11.9668350211295,3.23326515211326,-11.8094568448422));
#20098=CARTESIAN_POINT('Ctrl Pts',(13.8834175105647,2.99011502771357,-13.9072965714997));
#20099=CARTESIAN_POINT('Ctrl Pts',(15.8,2.74735768261531,-16.0050591347847));
#20100=CARTESIAN_POINT('Ctrl Pts',(10.0502525316942,3.414097226746,-9.64719632995103));
#20101=CARTESIAN_POINT('Ctrl Pts',(11.9668350211295,3.16465335082917,-11.7274687236956));
#20102=CARTESIAN_POINT('Ctrl Pts',(13.8834175105647,2.91499625447087,-13.8077428217682));
#20103=CARTESIAN_POINT('Ctrl Pts',(15.8,2.66555237855405,-15.8880152155128));
#20104=CARTESIAN_POINT('Ctrl Pts',(10.0502525316942,3.30251999207182,-9.53672408685997));
#20105=CARTESIAN_POINT('Ctrl Pts',(11.9668350211294,3.04246362184766,-11.5857749779899));
#20106=CARTESIAN_POINT('Ctrl Pts',(13.8834175105647,2.78215337892879,-13.6349367240444));
#20107=CARTESIAN_POINT('Ctrl Pts',(15.8,2.52209700870463,-15.6839876151744));
#20108=CARTESIAN_POINT('Ctrl Pts',(10.0502525316942,3.09139659750779,-9.36058107581316));
#20109=CARTESIAN_POINT('Ctrl Pts',(11.9668350211295,2.80829724126977,-11.357410148179));
#20110=CARTESIAN_POINT('Ctrl Pts',(13.8834175105647,2.52507603204706,-13.3541948572957));
#20111=CARTESIAN_POINT('Ctrl Pts',(15.8,2.24197667580905,-15.3510239296616));
#20112=CARTESIAN_POINT('Ctrl Pts',(10.0502525316942,2.94903314862294,-9.14733948977135));
#20113=CARTESIAN_POINT('Ctrl Pts',(11.9668350211294,2.65653626154119,-11.0909774008914));
#20114=CARTESIAN_POINT('Ctrl Pts',(13.8834175105647,2.36392896441619,-13.0346322911662));
#20115=CARTESIAN_POINT('Ctrl Pts',(15.8,2.07143207733444,-14.9782702022863));
#20116=CARTESIAN_POINT('Ctrl Pts',(10.0502525316942,2.83936642791008,-8.92650608260145));
#20117=CARTESIAN_POINT('Ctrl Pts',(11.9668350211294,2.54644119432443,-10.8177624863471));
#20118=CARTESIAN_POINT('Ctrl Pts',(13.8834175105648,2.2534334908895,-12.7090406610097));
#20119=CARTESIAN_POINT('Ctrl Pts',(15.8,1.96050825730386,-14.6002970647553));
#20120=CARTESIAN_POINT('Ctrl Pts',(10.0502525316942,2.80374461319022,-8.80866270544546));
#20121=CARTESIAN_POINT('Ctrl Pts',(11.9668350211294,2.51464388608039,-10.6741860277864));
#20122=CARTESIAN_POINT('Ctrl Pts',(13.8834175105647,2.22549660720977,-12.5396724561545));
#20123=CARTESIAN_POINT('Ctrl Pts',(15.8,1.93639588009993,-14.4051957784954));
#20124=CARTESIAN_POINT('Ctrl Pts',(10.0502525316942,2.78743136471945,-8.7276078365385));
#20125=CARTESIAN_POINT('Ctrl Pts',(11.9668350211294,2.50261311086535,-10.5761285330411));
#20126=CARTESIAN_POINT('Ctrl Pts',(13.8834175105647,2.21779485701124,-12.4246492295437));
#20127=CARTESIAN_POINT('Ctrl Pts',(15.8,1.93297660315714,-14.2731699260464));
#20128=CARTESIAN_POINT('Ctrl Pts',(15.8,1.93458023611785,-14.3165490635069));
#20129=CARTESIAN_POINT('Ctrl Pts',(15.8,1.93416388872989,-14.3078898665466));
#20130=CARTESIAN_POINT('Ctrl Pts',(15.8,1.93379536300002,-14.2992223526576));
#20131=CARTESIAN_POINT('Ctrl Pts',(15.8,1.93347464492456,-14.2905465237881));
#20132=CARTESIAN_POINT('Ctrl Pts',(15.8,1.93320172507161,-14.2818623815451));
#20133=CARTESIAN_POINT('Ctrl Pts',(15.8,1.93297660315714,-14.2731699260464));
#20134=CARTESIAN_POINT('Origin',(15.8,3.35534058166952,-14.6809722990553));
#20135=CARTESIAN_POINT('Ctrl Pts',(10.0502525316942,1.22531840158854,-10.6909231138624));
#20136=CARTESIAN_POINT('Ctrl Pts',(11.9668350211294,0.476385041699009,-12.7560692212929));
#20137=CARTESIAN_POINT('Ctrl Pts',(13.8834175105647,-0.272548318190526,
-14.8212153287235));
#20138=CARTESIAN_POINT('Ctrl Pts',(15.8,-1.02148167808006,-16.886361436154));
#20139=CARTESIAN_POINT('Ctrl Pts',(10.0502525316942,0.951811288039437,-10.6687583477967));
#20140=CARTESIAN_POINT('Ctrl Pts',(11.9668350211294,0.160771418505766,-12.7082628707158));
#20141=CARTESIAN_POINT('Ctrl Pts',(13.8834175105647,-0.630916858166454,
-14.7477045483503));
#20142=CARTESIAN_POINT('Ctrl Pts',(15.8,-1.42195672770012,-16.7872090712694));
#20143=CARTESIAN_POINT('Ctrl Pts',(10.0502525316942,0.53873797019293,-10.5909841198542));
#20144=CARTESIAN_POINT('Ctrl Pts',(11.9668350211294,-0.315735593698357,
-12.5832583421986));
#20145=CARTESIAN_POINT('Ctrl Pts',(13.8834175105647,-1.16942659814004,-14.5756107736058));
#20146=CARTESIAN_POINT('Ctrl Pts',(15.8,-2.02390016203133,-16.5678849959503));
#20147=CARTESIAN_POINT('Ctrl Pts',(10.0502525316942,0.350797420983484,-10.4118557126012));
#20148=CARTESIAN_POINT('Ctrl Pts',(11.9668350211294,-0.527317792292718,
-12.3552036734465));
#20149=CARTESIAN_POINT('Ctrl Pts',(13.8834175105647,-1.40583184426592,-14.2985259967778));
#20150=CARTESIAN_POINT('Ctrl Pts',(15.8,-2.28394705754213,-16.2418739576232));
#20151=CARTESIAN_POINT('Ctrl Pts',(10.0502525316942,0.276502431596342,-10.2498870013208));
#20152=CARTESIAN_POINT('Ctrl Pts',(11.9668350211294,-0.603405794214882,
-12.1559807242605));
#20153=CARTESIAN_POINT('Ctrl Pts',(13.8834175105647,-1.48361038150706,-14.0620012424206));
#20154=CARTESIAN_POINT('Ctrl Pts',(15.8,-2.36351860731828,-15.9680949653604));
#20155=CARTESIAN_POINT('Ctrl Pts',(10.0502525316942,0.193479460458701,-10.0905890686414));
#20156=CARTESIAN_POINT('Ctrl Pts',(11.9668350211294,-0.687106219194378,
-11.9589846875421));
#20157=CARTESIAN_POINT('Ctrl Pts',(13.8834175105647,-1.56802487912709,-13.8273908205778));
#20158=CARTESIAN_POINT('Ctrl Pts',(15.8,-2.44861055878017,-15.6957864394785));
#20159=CARTESIAN_POINT('Ctrl Pts',(10.0502525316942,0.0477779613143522,
-9.85767148446325));
#20160=CARTESIAN_POINT('Ctrl Pts',(11.9668350211294,-0.83847512310783,-11.6692901486065));
#20161=CARTESIAN_POINT('Ctrl Pts',(13.8834175105647,-1.72481200902093,-13.4808398643785));
#20162=CARTESIAN_POINT('Ctrl Pts',(15.8,-2.61106509344311,-15.2924585285217));
#20163=CARTESIAN_POINT('Ctrl Pts',(10.0502525316942,-0.0220599042734183,
-9.6109546595346));
#20164=CARTESIAN_POINT('Ctrl Pts',(11.9668350211294,-0.900879773662289,
-11.3690757684926));
#20165=CARTESIAN_POINT('Ctrl Pts',(13.8834175105647,-1.77979551853007,-13.1271782591657));
#20166=CARTESIAN_POINT('Ctrl Pts',(15.8,-2.65861538791894,-14.8852993681237));
#20167=CARTESIAN_POINT('Ctrl Pts',(10.0502525316942,-0.0579833517275581,
-9.36700900338232));
#20168=CARTESIAN_POINT('Ctrl Pts',(11.9668350211294,-0.920984711114089,
-11.07518337287));
#20169=CARTESIAN_POINT('Ctrl Pts',(13.8834175105647,-1.78409102238058,-12.7833535968728));
#20170=CARTESIAN_POINT('Ctrl Pts',(15.8,-2.64709238176712,-14.4915279663605));
#20171=CARTESIAN_POINT('Ctrl Pts',(10.0502525316942,-0.0555068892974584,
-9.243940799223));
#20172=CARTESIAN_POINT('Ctrl Pts',(11.9668350211294,-0.906948929192826,
-10.9288207869826));
#20173=CARTESIAN_POINT('Ctrl Pts',(13.8834175105647,-1.75838634306183,-12.6136545606744));
#20174=CARTESIAN_POINT('Ctrl Pts',(15.8,-2.6098283829572,-14.298534548434));
#20175=CARTESIAN_POINT('Ctrl Pts',(10.0502525316942,-0.0459743785884374,
-9.16181196696065));
#20176=CARTESIAN_POINT('Ctrl Pts',(11.9668350211294,-0.888076944549316,
-10.8318459401268));
#20177=CARTESIAN_POINT('Ctrl Pts',(13.8834175105647,-1.73017951051019,-12.501879913293));
#20178=CARTESIAN_POINT('Ctrl Pts',(15.8,-2.57228207647107,-14.1719138864591));
#20179=CARTESIAN_POINT('Ctrl Pts',(15.8,-2.58416182157067,-14.2136654476498));
#20180=CARTESIAN_POINT('Ctrl Pts',(15.8,-2.58188195244865,-14.2053014035364));
#20181=CARTESIAN_POINT('Ctrl Pts',(15.8,-2.57955403215479,-14.1969442272588));
#20182=CARTESIAN_POINT('Ctrl Pts',(15.8,-2.57717807460939,-14.1885939163425));
#20183=CARTESIAN_POINT('Ctrl Pts',(15.8,-2.57475408927931,-14.1802504694012));
#20184=CARTESIAN_POINT('Ctrl Pts',(15.8,-2.57228207647107,-14.1719138864591));
#20185=CARTESIAN_POINT('Origin',(15.8,-1.34555140976956,-14.999291632217));
#20186=CARTESIAN_POINT('Ctrl Pts',(10.0502525316942,-2.13832987737225,-10.5463163022605));
#20187=CARTESIAN_POINT('Ctrl Pts',(11.9668350211294,-3.48877307262933,-12.2789538289737));
#20188=CARTESIAN_POINT('Ctrl Pts',(13.8834175105647,-4.8392162678864,-14.0115913556869));
#20189=CARTESIAN_POINT('Ctrl Pts',(15.8,-6.18965946314348,-15.7442288824001));
#20190=CARTESIAN_POINT('Ctrl Pts',(10.0502525316942,-2.39160131057558,-10.4407180108925));
#20191=CARTESIAN_POINT('Ctrl Pts',(11.9668350211294,-3.77416649083142,-12.1359573145141));
#20192=CARTESIAN_POINT('Ctrl Pts',(13.8834175105647,-5.15732892266062,-13.8309364798931));
#20193=CARTESIAN_POINT('Ctrl Pts',(15.8,-6.53989410291645,-15.5261757835147));
#20194=CARTESIAN_POINT('Ctrl Pts',(10.0502525316942,-2.7604211119455,-10.2391038402362));
#20195=CARTESIAN_POINT('Ctrl Pts',(11.9668350211294,-4.18872035504581,-11.8698223691572));
#20196=CARTESIAN_POINT('Ctrl Pts',(13.8834175105647,-5.61629814839675,-13.5008577836237));
#20197=CARTESIAN_POINT('Ctrl Pts',(15.8,-7.04459739149706,-15.1315763125447));
#20198=CARTESIAN_POINT('Ctrl Pts',(10.0502525316942,-2.88380634898391,-10.0106660065973));
#20199=CARTESIAN_POINT('Ctrl Pts',(11.9668350211294,-4.31947109051326,-11.5875472242667));
#20200=CARTESIAN_POINT('Ctrl Pts',(13.8834175105647,-5.75550424110768,-13.1642822866715));
#20201=CARTESIAN_POINT('Ctrl Pts',(15.8,-7.19116898263704,-14.7411635043409));
#20202=CARTESIAN_POINT('Ctrl Pts',(10.0502525316942,-2.90441220847246,-9.83366631411429));
#20203=CARTESIAN_POINT('Ctrl Pts',(11.9668350211294,-4.33027001363173,-11.3745625747195));
#20204=CARTESIAN_POINT('Ctrl Pts',(13.8834175105647,-5.75638324902558,-12.9152995332973));
#20205=CARTESIAN_POINT('Ctrl Pts',(15.8,-7.18224105418486,-14.4561957939025));
#20206=CARTESIAN_POINT('Ctrl Pts',(10.0502525316941,-2.93414649567711,-9.65650945139357));
#20207=CARTESIAN_POINT('Ctrl Pts',(11.9668350211294,-4.34899924292338,-11.1613433397504));
#20208=CARTESIAN_POINT('Ctrl Pts',(13.8834175105647,-5.76416819477548,-12.6660861533134));
#20209=CARTESIAN_POINT('Ctrl Pts',(15.8,-7.17902094202174,-14.1709200416702));
#20210=CARTESIAN_POINT('Ctrl Pts',(10.0502525316942,-3.00074150798573,-9.38996734645582));
#20211=CARTESIAN_POINT('Ctrl Pts',(11.9668350211294,-4.40343923355922,-10.8390518176275));
#20212=CARTESIAN_POINT('Ctrl Pts',(13.8834175105647,-5.80619247524441,-12.2880463890102));
#20213=CARTESIAN_POINT('Ctrl Pts',(15.8,-7.20889020081791,-13.7371308601818));
#20214=CARTESIAN_POINT('Ctrl Pts',(10.0502525316942,-2.99092345166592,-9.13374448664767));
#20215=CARTESIAN_POINT('Ctrl Pts',(11.9668350211294,-4.37002011593521,-10.5342467491227));
#20216=CARTESIAN_POINT('Ctrl Pts',(13.8834175105647,-5.74920012742636,-11.9347028120052));
#20217=CARTESIAN_POINT('Ctrl Pts',(15.8,-7.12829679169565,-13.3352050744803));
#20218=CARTESIAN_POINT('Ctrl Pts',(10.0502525316942,-2.94970615383951,-8.89063737063807));
#20219=CARTESIAN_POINT('Ctrl Pts',(11.9668350211294,-4.29832412978306,-10.2485256494886));
#20220=CARTESIAN_POINT('Ctrl Pts',(13.8834175105647,-5.64703889510256,-11.6063785007713));
#20221=CARTESIAN_POINT('Ctrl Pts',(15.8,-6.99565687104611,-12.9642667796218));
#20222=CARTESIAN_POINT('Ctrl Pts',(10.0502525316942,-2.90932499072146,-8.77435756124985));
#20223=CARTESIAN_POINT('Ctrl Pts',(11.9668350211294,-4.23975104071156,-10.113663592731));
#20224=CARTESIAN_POINT('Ctrl Pts',(13.8834175105647,-5.57015841015682,-11.4529271015425));
#20225=CARTESIAN_POINT('Ctrl Pts',(15.8,-6.90058446014692,-12.7922331330237));
#20226=CARTESIAN_POINT('Ctrl Pts',(10.0502525316942,-2.87487982939776,-8.69919410795919));
#20227=CARTESIAN_POINT('Ctrl Pts',(11.9668350211294,-4.19183584103558,-10.0272667966845));
#20228=CARTESIAN_POINT('Ctrl Pts',(13.8834175105647,-5.5087918526734,-11.3553394854098));
#20229=CARTESIAN_POINT('Ctrl Pts',(15.8,-6.82574786431122,-12.6834121741351));
#20230=CARTESIAN_POINT('Ctrl Pts',(15.8,-6.84994811524973,-12.7194492253464));
#20231=CARTESIAN_POINT('Ctrl Pts',(15.8,-6.84519519909218,-12.7121990649934));
#20232=CARTESIAN_POINT('Ctrl Pts',(15.8,-6.84039870583253,-12.7049702849691));
#20233=CARTESIAN_POINT('Ctrl Pts',(15.8,-6.83555864794507,-12.6977628786185));
#20234=CARTESIAN_POINT('Ctrl Pts',(15.8,-6.83067503400497,-12.6905768416977));
#20235=CARTESIAN_POINT('Ctrl Pts',(15.8,-6.82574786431122,-12.6834121741351));
#20236=CARTESIAN_POINT('Origin',(15.8,-5.91473145421246,-13.8493757942074));
#20237=CARTESIAN_POINT('Ctrl Pts',(10.0502525316942,-5.29266352931554,-9.36936257048691));
#20238=CARTESIAN_POINT('Ctrl Pts',(11.9668350211294,-7.11242577089738,-10.5998888833726));
#20239=CARTESIAN_POINT('Ctrl Pts',(13.8834175105647,-8.93218801247923,-11.8304151962582));
#20240=CARTESIAN_POINT('Ctrl Pts',(15.8,-10.7519502540611,-13.0609415091439));
#20241=CARTESIAN_POINT('Ctrl Pts',(10.0502525316942,-5.50090730964532,-9.19066745032221));
#20242=CARTESIAN_POINT('Ctrl Pts',(11.9668350211294,-7.33966268788185,-10.3756997001811));
#20243=CARTESIAN_POINT('Ctrl Pts',(13.8834175105647,-9.17890569898124,-11.5602999829831));
#20244=CARTESIAN_POINT('Ctrl Pts',(15.8,-11.0176610772178,-12.745332232842));
#20245=CARTESIAN_POINT('Ctrl Pts',(10.0502525316942,-5.78937538435653,-8.88494866314842));
#20246=CARTESIAN_POINT('Ctrl Pts',(11.9668350211294,-7.65168842520523,-9.99448540715111));
#20247=CARTESIAN_POINT('Ctrl Pts',(13.8834175105647,-9.51341402508183,-11.104545703274));
#20248=CARTESIAN_POINT('Ctrl Pts',(15.8,-11.3757270659305,-12.2140824472766));
#20249=CARTESIAN_POINT('Ctrl Pts',(10.0502525316942,-5.83613263565859,-8.62956238511758));
#20250=CARTESIAN_POINT('Ctrl Pts',(11.9668350211294,-7.68881403767578,-9.68562073924798));
#20251=CARTESIAN_POINT('Ctrl Pts',(13.8834175105647,-9.54180236671465,-10.7414245752752));
#20252=CARTESIAN_POINT('Ctrl Pts',(15.8,-11.3944837687318,-11.7974829294056));
#20253=CARTESIAN_POINT('Ctrl Pts',(10.0502525316942,-5.80103525788045,-8.45485763321061));
#20254=CARTESIAN_POINT('Ctrl Pts',(11.9668350211294,-7.6332697458833,-9.47972276943763));
#20255=CARTESIAN_POINT('Ctrl Pts',(13.8834175105647,-9.46570011434025,-10.5043553237743));
#20256=CARTESIAN_POINT('Ctrl Pts',(15.8,-11.2979346023431,-11.5292204600013));
#20257=CARTESIAN_POINT('Ctrl Pts',(10.0502525316941,-5.77456941285602,-8.27718317134364));
#20258=CARTESIAN_POINT('Ctrl Pts',(11.9668350211294,-7.58519358293626,-9.27115170336996));
#20259=CARTESIAN_POINT('Ctrl Pts',(13.8834175105647,-9.39609248134292,-10.2649338319875));
#20260=CARTESIAN_POINT('Ctrl Pts',(15.8,-11.2067166514232,-11.2589023640139));
#20261=CARTESIAN_POINT('Ctrl Pts',(10.0502525316942,-5.75553891274799,-8.0031076613001));
#20262=CARTESIAN_POINT('Ctrl Pts',(11.9668350211295,-7.53737545292393,-8.94781145509674));
#20263=CARTESIAN_POINT('Ctrl Pts',(13.8834175105647,-9.31923862861202,-9.89241088219744));
#20264=CARTESIAN_POINT('Ctrl Pts',(15.8,-11.101075168788,-10.8371146759941));
#20265=CARTESIAN_POINT('Ctrl Pts',(10.0502525316942,-5.66702291215723,-7.76245969237558));
#20266=CARTESIAN_POINT('Ctrl Pts',(11.9668350211294,-7.4114007810768,-8.66825218904355));
#20267=CARTESIAN_POINT('Ctrl Pts',(13.8834175105647,-9.1558448117796,-9.57397375447812));
#20268=CARTESIAN_POINT('Ctrl Pts',(15.8,-10.9002226806992,-10.4797662511461));
#20269=CARTESIAN_POINT('Ctrl Pts',(10.0502525316942,-5.55269814935977,-7.54398815168985));
#20270=CARTESIAN_POINT('Ctrl Pts',(11.9668350211294,-7.25492061800102,-8.41867077420536));
#20271=CARTESIAN_POINT('Ctrl Pts',(13.8834175105647,-8.95722517253276,-9.29328875951756));
#20272=CARTESIAN_POINT('Ctrl Pts',(15.8,-10.659447641174,-10.1679713820331));
#20273=CARTESIAN_POINT('Ctrl Pts',(10.0502525316942,-5.47835809159451,-7.44587907063767));
#20274=CARTESIAN_POINT('Ctrl Pts',(11.9668350211294,-7.15753678028296,-8.30851053998513));
#20275=CARTESIAN_POINT('Ctrl Pts',(13.8834175105647,-8.83668456248994,-9.17110734047641));
#20276=CARTESIAN_POINT('Ctrl Pts',(15.8,-10.5158632511784,-10.0337388098239));
#20277=CARTESIAN_POINT('Ctrl Pts',(10.0502525316942,-5.42237201204004,-7.38503851882133));
#20278=CARTESIAN_POINT('Ctrl Pts',(11.9668350211294,-7.08526863916361,-8.24114891510682));
#20279=CARTESIAN_POINT('Ctrl Pts',(13.8834175105647,-8.74816526628719,-9.09725931139231));
#20280=CARTESIAN_POINT('Ctrl Pts',(15.8,-10.4110618934108,-9.95336970767779));
#20281=CARTESIAN_POINT('Ctrl Pts',(15.8,-10.4452137610133,-9.9801646912522));
#20282=CARTESIAN_POINT('Ctrl Pts',(15.8,-10.4384530463692,-9.97473811086981));
#20283=CARTESIAN_POINT('Ctrl Pts',(15.8,-10.4316574943231,-9.96934533045351));
#20284=CARTESIAN_POINT('Ctrl Pts',(15.8,-10.4248271146823,-9.96398633981914));
#20285=CARTESIAN_POINT('Ctrl Pts',(15.8,-10.4179619142908,-9.95866113228077));
#20286=CARTESIAN_POINT('Ctrl Pts',(15.8,-10.4110618934108,-9.95336970767779));
#20287=CARTESIAN_POINT('Origin',(15.8,-9.90493637355978,-11.3437865591856));
#20288=CARTESIAN_POINT('Ctrl Pts',(10.0502525316942,-7.92891439885425,-7.2752703501265));
#20289=CARTESIAN_POINT('Ctrl Pts',(11.9668350211294,-10.0398646795257,-7.88323296009842));
#20290=CARTESIAN_POINT('Ctrl Pts',(13.8834175105647,-12.1508149601973,-8.49119557007034));
#20291=CARTESIAN_POINT('Ctrl Pts',(15.8,-14.2617652408688,-9.09915818004226));
#20292=CARTESIAN_POINT('Ctrl Pts',(10.0502525316942,-8.07174617417205,-7.04097032456894));
#20293=CARTESIAN_POINT('Ctrl Pts',(11.9668350211294,-10.186749261509,-7.59972129962698));
#20294=CARTESIAN_POINT('Ctrl Pts',(13.8834175105647,-12.3019395333854,-8.15813578620935));
#20295=CARTESIAN_POINT('Ctrl Pts',(15.8,-14.4169426207224,-8.71688676126738));
#20296=CARTESIAN_POINT('Ctrl Pts',(10.0502525316942,-8.25126590443755,-6.66138127597024));
#20297=CARTESIAN_POINT('Ctrl Pts',(11.9668350211294,-10.365200404417,-7.14127838379811));
#20298=CARTESIAN_POINT('Ctrl Pts',(13.8834175105647,-12.4788866778492,-7.62165928459738));
#20299=CARTESIAN_POINT('Ctrl Pts',(15.8,-14.5928211778286,-8.10155639242525));
#20300=CARTESIAN_POINT('Ctrl Pts',(10.0502525316942,-8.22079862024226,-6.42930419296208));
#20301=CARTESIAN_POINT('Ctrl Pts',(11.9668350211294,-10.3118069242151,-6.86580395314969));
#20302=CARTESIAN_POINT('Ctrl Pts',(13.8834175105647,-12.4027801127282,-7.30234839548021));
#20303=CARTESIAN_POINT('Ctrl Pts',(15.8,-14.493788416701,-7.73884815566781));
#20304=CARTESIAN_POINT('Ctrl Pts',(10.0502525316942,-8.16221173215364,-6.30697938690416));
#20305=CARTESIAN_POINT('Ctrl Pts',(11.9668350211294,-10.2323186327506,-6.72434771418858));
#20306=CARTESIAN_POINT('Ctrl Pts',(13.8834175105647,-12.3026176380752,-7.1413715062851));
#20307=CARTESIAN_POINT('Ctrl Pts',(15.8,-14.3727245386721,-7.55873983356951));
#20308=CARTESIAN_POINT('Ctrl Pts',(10.0502525316942,-8.12000643506485,-6.22815403351084));
#20309=CARTESIAN_POINT('Ctrl Pts',(11.9668350211294,-10.1755454476056,-6.63375833246636));
#20310=CARTESIAN_POINT('Ctrl Pts',(13.8834175105647,-12.2311493413123,-7.03916552489902));
#20311=CARTESIAN_POINT('Ctrl Pts',(15.8,-14.2866883538531,-7.44476982385454));
#20312=CARTESIAN_POINT('Ctrl Pts',(10.0502525316942,-8.04942040067478,-6.08789997184504));
#20313=CARTESIAN_POINT('Ctrl Pts',(11.9668350211294,-10.0785454407991,-6.47376321403759));
#20314=CARTESIAN_POINT('Ctrl Pts',(13.8834175105647,-12.1078515605739,-6.85942462405723));
#20315=CARTESIAN_POINT('Ctrl Pts',(15.8,-14.1369766006982,-7.24528786624978));
#20316=CARTESIAN_POINT('Ctrl Pts',(10.0502525316942,-7.94713925110583,-5.83267830770086));
#20317=CARTESIAN_POINT('Ctrl Pts',(11.9668350211294,-9.93371906448112,-6.18048893841474));
#20318=CARTESIAN_POINT('Ctrl Pts',(13.8834175105647,-11.920292369998,-6.52817426230451));
#20319=CARTESIAN_POINT('Ctrl Pts',(15.8,-13.9068721833733,-6.87598489301839));
#20320=CARTESIAN_POINT('Ctrl Pts',(10.0502525316942,-7.78832910259187,-5.63138575926579));
#20321=CARTESIAN_POINT('Ctrl Pts',(11.9668350211294,-9.7272251121909,-5.95382183425815));
#20322=CARTESIAN_POINT('Ctrl Pts',(13.8834175105647,-11.6661698490829,-6.27616146093385));
#20323=CARTESIAN_POINT('Ctrl Pts',(15.8,-13.605065858682,-6.59859753592622));
#20324=CARTESIAN_POINT('Ctrl Pts',(10.0502525316942,-7.61219406851115,-5.45884429554414));
#20325=CARTESIAN_POINT('Ctrl Pts',(11.9668350211294,-9.50140467053763,-5.76468621283309));
#20326=CARTESIAN_POINT('Ctrl Pts',(13.8834175105648,-11.3906602079427,-6.07045912241827));
#20327=CARTESIAN_POINT('Ctrl Pts',(15.8,-13.2798708099692,-6.37630103970722));
#20328=CARTESIAN_POINT('Ctrl Pts',(10.0502525316942,-7.51113133249701,-5.38854605810145));
#20329=CARTESIAN_POINT('Ctrl Pts',(11.9668350211294,-9.37468648227302,-5.69007333772413));
#20330=CARTESIAN_POINT('Ctrl Pts',(13.8834175105647,-11.238220929081,-5.99154494312677));
#20331=CARTESIAN_POINT('Ctrl Pts',(15.8,-13.101776078857,-6.29307222274945));
#20332=CARTESIAN_POINT('Ctrl Pts',(10.0502525316942,-7.43908464225652,-5.34798390487229));
#20333=CARTESIAN_POINT('Ctrl Pts',(11.9668350211294,-9.28514597692092,-5.64832995825767));
#20334=CARTESIAN_POINT('Ctrl Pts',(13.8834175105647,-11.1312073115853,-5.94867601164304));
#20335=CARTESIAN_POINT('Ctrl Pts',(15.8,-12.9772686462497,-6.24902206502841));
#20336=CARTESIAN_POINT('Ctrl Pts',(15.8,-13.0180291077652,-6.26395210128206));
#20337=CARTESIAN_POINT('Ctrl Pts',(15.8,-13.0099223804886,-6.26088029236732));
#20338=CARTESIAN_POINT('Ctrl Pts',(15.8,-13.0017929656379,-6.25785139447984));
#20339=CARTESIAN_POINT('Ctrl Pts',(15.8,-12.993640869393,-6.25486539490331));
#20340=CARTESIAN_POINT('Ctrl Pts',(15.8,-12.985466096197,-6.25192228516409));
#20341=CARTESIAN_POINT('Ctrl Pts',(15.8,-12.9772686462497,-6.24902206502841));
#20342=CARTESIAN_POINT('Origin',(15.8,-12.9255771089134,-7.7277884589423));
#20343=CARTESIAN_POINT('Ctrl Pts',(10.0502525316942,-9.78902788303806,-4.46902397810655));
#20344=CARTESIAN_POINT('Ctrl Pts',(11.9668350211294,-11.9845316814717,-4.39491126897609));
#20345=CARTESIAN_POINT('Ctrl Pts',(13.8834175105647,-14.1800354799052,-4.32079855984563));
#20346=CARTESIAN_POINT('Ctrl Pts',(15.8,-16.3755392783388,-4.24668585071518));
#20347=CARTESIAN_POINT('Ctrl Pts',(10.0502525316942,-9.8524662840083,-4.20205396612197));
#20348=CARTESIAN_POINT('Ctrl Pts',(11.9668350211294,-12.036617299121,-4.07988582479457));
#20349=CARTESIAN_POINT('Ctrl Pts',(13.8834175105647,-14.2208423566523,-3.95733982070599));
#20350=CARTESIAN_POINT('Ctrl Pts',(15.8,-16.404993371765,-3.83517167937859));
#20351=CARTESIAN_POINT('Ctrl Pts',(10.0502525316942,-9.90590216992165,-3.78556561092159));
#20352=CARTESIAN_POINT('Ctrl Pts',(11.9668350211295,-12.0646697130184,-3.58873319698333));
#20353=CARTESIAN_POINT('Ctrl Pts',(13.8834175105647,-14.2233509855394,-3.39243568541409));
#20354=CARTESIAN_POINT('Ctrl Pts',(15.8,-16.3821185286362,-3.19560327147583));
#20355=CARTESIAN_POINT('Ctrl Pts',(10.0502525316942,-9.80521299123422,-3.57425782911966));
#20356=CARTESIAN_POINT('Ctrl Pts',(11.9668350211295,-11.9287659082934,-3.34323666910061));
#20357=CARTESIAN_POINT('Ctrl Pts',(13.8834175105647,-14.0522999619539,-3.11226431322854));
#20358=CARTESIAN_POINT('Ctrl Pts',(15.8,-16.1758528790132,-2.8812431532095));
#20359=CARTESIAN_POINT('Ctrl Pts',(10.0502525316942,-9.71169428155716,-3.47602249721152));
#20360=CARTESIAN_POINT('Ctrl Pts',(11.9668350211295,-11.8094568448422,-3.23326515211326));
#20361=CARTESIAN_POINT('Ctrl Pts',(13.8834175105647,-13.9072965714997,-2.99011502771357));
#20362=CARTESIAN_POINT('Ctrl Pts',(15.8,-16.0050591347847,-2.74735768261532));
#20363=CARTESIAN_POINT('Ctrl Pts',(10.0502525316942,-9.64719632995103,-3.414097226746));
#20364=CARTESIAN_POINT('Ctrl Pts',(11.9668350211295,-11.7274687236956,-3.16465335082917));
#20365=CARTESIAN_POINT('Ctrl Pts',(13.8834175105647,-13.8077428217682,-2.91499625447087));
#20366=CARTESIAN_POINT('Ctrl Pts',(15.8,-15.8880152155128,-2.66555237855405));
#20367=CARTESIAN_POINT('Ctrl Pts',(10.0502525316942,-9.53672408685997,-3.30251999207182));
#20368=CARTESIAN_POINT('Ctrl Pts',(11.9668350211294,-11.58577497799,-3.04246362184766));
#20369=CARTESIAN_POINT('Ctrl Pts',(13.8834175105647,-13.6349367240444,-2.78215337892879));
#20370=CARTESIAN_POINT('Ctrl Pts',(15.8,-15.6839876151744,-2.52209700870464));
#20371=CARTESIAN_POINT('Ctrl Pts',(10.0502525316942,-9.36058107581316,-3.09139659750779));
#20372=CARTESIAN_POINT('Ctrl Pts',(11.9668350211295,-11.357410148179,-2.80829724126978));
#20373=CARTESIAN_POINT('Ctrl Pts',(13.8834175105647,-13.3541948572957,-2.52507603204706));
#20374=CARTESIAN_POINT('Ctrl Pts',(15.8,-15.3510239296616,-2.24197667580905));
#20375=CARTESIAN_POINT('Ctrl Pts',(10.0502525316942,-9.14733948977135,-2.94903314862294));
#20376=CARTESIAN_POINT('Ctrl Pts',(11.9668350211294,-11.0909774008914,-2.65653626154118));
#20377=CARTESIAN_POINT('Ctrl Pts',(13.8834175105647,-13.0346322911662,-2.3639289644162));
#20378=CARTESIAN_POINT('Ctrl Pts',(15.8,-14.9782702022863,-2.07143207733444));
#20379=CARTESIAN_POINT('Ctrl Pts',(10.0502525316942,-8.92650608260145,-2.83936642791009));
#20380=CARTESIAN_POINT('Ctrl Pts',(11.9668350211294,-10.8177624863471,-2.54644119432444));
#20381=CARTESIAN_POINT('Ctrl Pts',(13.8834175105648,-12.7090406610097,-2.2534334908895));
#20382=CARTESIAN_POINT('Ctrl Pts',(15.8,-14.6002970647553,-1.96050825730385));
#20383=CARTESIAN_POINT('Ctrl Pts',(10.0502525316942,-8.80866270544546,-2.80374461319022));
#20384=CARTESIAN_POINT('Ctrl Pts',(11.9668350211294,-10.6741860277864,-2.51464388608039));
#20385=CARTESIAN_POINT('Ctrl Pts',(13.8834175105647,-12.5396724561545,-2.22549660720977));
#20386=CARTESIAN_POINT('Ctrl Pts',(15.8,-14.4051957784954,-1.93639588009993));
#20387=CARTESIAN_POINT('Ctrl Pts',(10.0502525316942,-8.7276078365385,-2.78743136471945));
#20388=CARTESIAN_POINT('Ctrl Pts',(11.9668350211294,-10.5761285330411,-2.50261311086535));
#20389=CARTESIAN_POINT('Ctrl Pts',(13.8834175105647,-12.4246492295437,-2.21779485701124));
#20390=CARTESIAN_POINT('Ctrl Pts',(15.8,-14.2731699260464,-1.93297660315714));
#20391=CARTESIAN_POINT('Ctrl Pts',(15.8,-14.3165490635069,-1.93458023611785));
#20392=CARTESIAN_POINT('Ctrl Pts',(15.8,-14.3078898665466,-1.93416388872989));
#20393=CARTESIAN_POINT('Ctrl Pts',(15.8,-14.2992223526576,-1.93379536300002));
#20394=CARTESIAN_POINT('Ctrl Pts',(15.8,-14.2905465237881,-1.93347464492456));
#20395=CARTESIAN_POINT('Ctrl Pts',(15.8,-14.2818623815451,-1.93320172507161));
#20396=CARTESIAN_POINT('Ctrl Pts',(15.8,-14.2731699260464,-1.93297660315714));
#20397=CARTESIAN_POINT('Origin',(15.8,-14.6809722990553,-3.35534058166953));
#20398=CARTESIAN_POINT('Ctrl Pts',(10.0502525316942,-10.6909231138624,-1.22531840158854));
#20399=CARTESIAN_POINT('Ctrl Pts',(11.9668350211294,-12.7560692212929,-0.47638504169901));
#20400=CARTESIAN_POINT('Ctrl Pts',(13.8834175105647,-14.8212153287235,0.272548318190525));
#20401=CARTESIAN_POINT('Ctrl Pts',(15.8,-16.886361436154,1.02148167808006));
#20402=CARTESIAN_POINT('Ctrl Pts',(10.0502525316942,-10.6687583477967,-0.951811288039438));
#20403=CARTESIAN_POINT('Ctrl Pts',(11.9668350211294,-12.7082628707158,-0.160771418505767));
#20404=CARTESIAN_POINT('Ctrl Pts',(13.8834175105647,-14.7477045483503,0.630916858166453));
#20405=CARTESIAN_POINT('Ctrl Pts',(15.8,-16.7872090712694,1.42195672770012));
#20406=CARTESIAN_POINT('Ctrl Pts',(10.0502525316942,-10.5909841198542,-0.538737970192931));
#20407=CARTESIAN_POINT('Ctrl Pts',(11.9668350211295,-12.5832583421986,0.315735593698358));
#20408=CARTESIAN_POINT('Ctrl Pts',(13.8834175105647,-14.5756107736058,1.16942659814004));
#20409=CARTESIAN_POINT('Ctrl Pts',(15.8,-16.5678849959503,2.02390016203133));
#20410=CARTESIAN_POINT('Ctrl Pts',(10.0502525316942,-10.4118557126012,-0.350797420983485));
#20411=CARTESIAN_POINT('Ctrl Pts',(11.9668350211295,-12.3552036734465,0.527317792292715));
#20412=CARTESIAN_POINT('Ctrl Pts',(13.8834175105647,-14.2985259967778,1.40583184426593));
#20413=CARTESIAN_POINT('Ctrl Pts',(15.8,-16.2418739576232,2.28394705754213));
#20414=CARTESIAN_POINT('Ctrl Pts',(10.0502525316942,-10.2498870013208,-0.276502431596343));
#20415=CARTESIAN_POINT('Ctrl Pts',(11.9668350211295,-12.1559807242605,0.603405794214881));
#20416=CARTESIAN_POINT('Ctrl Pts',(13.8834175105647,-14.0620012424206,1.48361038150706));
#20417=CARTESIAN_POINT('Ctrl Pts',(15.8,-15.9680949653604,2.36351860731828));
#20418=CARTESIAN_POINT('Ctrl Pts',(10.0502525316942,-10.0905890686414,-0.193479460458702));
#20419=CARTESIAN_POINT('Ctrl Pts',(11.9668350211294,-11.9589846875421,0.687106219194376));
#20420=CARTESIAN_POINT('Ctrl Pts',(13.8834175105647,-13.8273908205778,1.56802487912709));
#20421=CARTESIAN_POINT('Ctrl Pts',(15.8,-15.6957864394785,2.44861055878017));
#20422=CARTESIAN_POINT('Ctrl Pts',(10.0502525316942,-9.85767148446325,-0.0477779613143529));
#20423=CARTESIAN_POINT('Ctrl Pts',(11.9668350211294,-11.6692901486065,0.83847512310783));
#20424=CARTESIAN_POINT('Ctrl Pts',(13.8834175105647,-13.4808398643785,1.72481200902093));
#20425=CARTESIAN_POINT('Ctrl Pts',(15.8,-15.2924585285217,2.61106509344311));
#20426=CARTESIAN_POINT('Ctrl Pts',(10.0502525316942,-9.61095465953459,0.0220599042734176));
#20427=CARTESIAN_POINT('Ctrl Pts',(11.9668350211294,-11.3690757684926,0.900879773662287));
#20428=CARTESIAN_POINT('Ctrl Pts',(13.8834175105647,-13.1271782591657,1.77979551853006));
#20429=CARTESIAN_POINT('Ctrl Pts',(15.8,-14.8852993681237,2.65861538791893));
#20430=CARTESIAN_POINT('Ctrl Pts',(10.0502525316942,-9.36700900338232,0.0579833517275573));
#20431=CARTESIAN_POINT('Ctrl Pts',(11.9668350211294,-11.07518337287,0.92098471111409));
#20432=CARTESIAN_POINT('Ctrl Pts',(13.8834175105647,-12.7833535968728,1.78409102238058));
#20433=CARTESIAN_POINT('Ctrl Pts',(15.8,-14.4915279663605,2.64709238176711));
#20434=CARTESIAN_POINT('Ctrl Pts',(10.0502525316942,-9.243940799223,0.0555068892974579));
#20435=CARTESIAN_POINT('Ctrl Pts',(11.9668350211294,-10.9288207869826,0.906948929192824));
#20436=CARTESIAN_POINT('Ctrl Pts',(13.8834175105647,-12.6136545606744,1.75838634306183));
#20437=CARTESIAN_POINT('Ctrl Pts',(15.8,-14.298534548434,2.6098283829572));
#20438=CARTESIAN_POINT('Ctrl Pts',(10.0502525316942,-9.16181196696065,0.0459743785884369));
#20439=CARTESIAN_POINT('Ctrl Pts',(11.9668350211294,-10.8318459401268,0.888076944549315));
#20440=CARTESIAN_POINT('Ctrl Pts',(13.8834175105647,-12.501879913293,1.73017951051019));
#20441=CARTESIAN_POINT('Ctrl Pts',(15.8,-14.1719138864591,2.57228207647107));
#20442=CARTESIAN_POINT('Ctrl Pts',(15.8,-14.2136654476498,2.58416182157067));
#20443=CARTESIAN_POINT('Ctrl Pts',(15.8,-14.2053014035364,2.58188195244865));
#20444=CARTESIAN_POINT('Ctrl Pts',(15.8,-14.1969442272588,2.57955403215479));
#20445=CARTESIAN_POINT('Ctrl Pts',(15.8,-14.1885939163425,2.57717807460939));
#20446=CARTESIAN_POINT('Ctrl Pts',(15.8,-14.1802504694012,2.57475408927931));
#20447=CARTESIAN_POINT('Ctrl Pts',(15.8,-14.1719138864591,2.57228207647107));
#20448=CARTESIAN_POINT('Origin',(15.8,-14.999291632217,1.34555140976956));
#20449=CARTESIAN_POINT('Ctrl Pts',(10.0502525316942,-10.5463163022605,2.13832987737225));
#20450=CARTESIAN_POINT('Ctrl Pts',(11.9668350211294,-12.2789538289737,3.48877307262933));
#20451=CARTESIAN_POINT('Ctrl Pts',(13.8834175105647,-14.0115913556869,4.8392162678864));
#20452=CARTESIAN_POINT('Ctrl Pts',(15.8,-15.7442288824001,6.18965946314348));
#20453=CARTESIAN_POINT('Ctrl Pts',(10.0502525316942,-10.4407180108925,2.39160131057558));
#20454=CARTESIAN_POINT('Ctrl Pts',(11.9668350211294,-12.1359573145141,3.77416649083142));
#20455=CARTESIAN_POINT('Ctrl Pts',(13.8834175105647,-13.8309364798931,5.15732892266062));
#20456=CARTESIAN_POINT('Ctrl Pts',(15.8,-15.5261757835147,6.53989410291645));
#20457=CARTESIAN_POINT('Ctrl Pts',(10.0502525316942,-10.2391038402362,2.76042111194549));
#20458=CARTESIAN_POINT('Ctrl Pts',(11.9668350211294,-11.8698223691572,4.18872035504581));
#20459=CARTESIAN_POINT('Ctrl Pts',(13.8834175105647,-13.5008577836237,5.61629814839673));
#20460=CARTESIAN_POINT('Ctrl Pts',(15.8,-15.1315763125447,7.04459739149705));
#20461=CARTESIAN_POINT('Ctrl Pts',(10.0502525316942,-10.0106660065973,2.88380634898392));
#20462=CARTESIAN_POINT('Ctrl Pts',(11.9668350211294,-11.5875472242667,4.31947109051328));
#20463=CARTESIAN_POINT('Ctrl Pts',(13.8834175105647,-13.1642822866715,5.75550424110768));
#20464=CARTESIAN_POINT('Ctrl Pts',(15.8,-14.7411635043409,7.19116898263704));
#20465=CARTESIAN_POINT('Ctrl Pts',(10.0502525316942,-9.83366631411429,2.90441220847246));
#20466=CARTESIAN_POINT('Ctrl Pts',(11.9668350211294,-11.3745625747195,4.33027001363174));
#20467=CARTESIAN_POINT('Ctrl Pts',(13.8834175105647,-12.9152995332973,5.75638324902558));
#20468=CARTESIAN_POINT('Ctrl Pts',(15.8,-14.4561957939025,7.18224105418486));
#20469=CARTESIAN_POINT('Ctrl Pts',(10.0502525316941,-9.65650945139357,2.93414649567711));
#20470=CARTESIAN_POINT('Ctrl Pts',(11.9668350211294,-11.1613433397504,4.34899924292338));
#20471=CARTESIAN_POINT('Ctrl Pts',(13.8834175105647,-12.6660861533134,5.76416819477547));
#20472=CARTESIAN_POINT('Ctrl Pts',(15.8,-14.1709200416702,7.17902094202174));
#20473=CARTESIAN_POINT('Ctrl Pts',(10.0502525316942,-9.38996734645582,3.00074150798572));
#20474=CARTESIAN_POINT('Ctrl Pts',(11.9668350211294,-10.8390518176275,4.40343923355921));
#20475=CARTESIAN_POINT('Ctrl Pts',(13.8834175105647,-12.2880463890101,5.8061924752444));
#20476=CARTESIAN_POINT('Ctrl Pts',(15.8,-13.7371308601818,7.20889020081789));
#20477=CARTESIAN_POINT('Ctrl Pts',(10.0502525316942,-9.13374448664767,2.99092345166592));
#20478=CARTESIAN_POINT('Ctrl Pts',(11.9668350211294,-10.5342467491227,4.37002011593521));
#20479=CARTESIAN_POINT('Ctrl Pts',(13.8834175105647,-11.9347028120052,5.74920012742636));
#20480=CARTESIAN_POINT('Ctrl Pts',(15.8,-13.3352050744802,7.12829679169565));
#20481=CARTESIAN_POINT('Ctrl Pts',(10.0502525316942,-8.89063737063807,2.94970615383951));
#20482=CARTESIAN_POINT('Ctrl Pts',(11.9668350211294,-10.2485256494886,4.29832412978306));
#20483=CARTESIAN_POINT('Ctrl Pts',(13.8834175105647,-11.6063785007713,5.64703889510258));
#20484=CARTESIAN_POINT('Ctrl Pts',(15.8,-12.9642667796218,6.99565687104613));
#20485=CARTESIAN_POINT('Ctrl Pts',(10.0502525316942,-8.77435756124986,2.90932499072146));
#20486=CARTESIAN_POINT('Ctrl Pts',(11.9668350211294,-10.113663592731,4.23975104071156));
#20487=CARTESIAN_POINT('Ctrl Pts',(13.8834175105647,-11.4529271015425,5.57015841015681));
#20488=CARTESIAN_POINT('Ctrl Pts',(15.8,-12.7922331330237,6.90058446014691));
#20489=CARTESIAN_POINT('Ctrl Pts',(10.0502525316942,-8.69919410795919,2.87487982939776));
#20490=CARTESIAN_POINT('Ctrl Pts',(11.9668350211294,-10.0272667966845,4.19183584103558));
#20491=CARTESIAN_POINT('Ctrl Pts',(13.8834175105647,-11.3553394854098,5.5087918526734));
#20492=CARTESIAN_POINT('Ctrl Pts',(15.8,-12.6834121741351,6.82574786431122));
#20493=CARTESIAN_POINT('Ctrl Pts',(15.8,-12.7194492253464,6.84994811524973));
#20494=CARTESIAN_POINT('Ctrl Pts',(15.8,-12.7121990649934,6.84519519909218));
#20495=CARTESIAN_POINT('Ctrl Pts',(15.8,-12.7049702849691,6.84039870583253));
#20496=CARTESIAN_POINT('Ctrl Pts',(15.8,-12.6977628786185,6.83555864794507));
#20497=CARTESIAN_POINT('Ctrl Pts',(15.8,-12.6905768416977,6.83067503400497));
#20498=CARTESIAN_POINT('Ctrl Pts',(15.8,-12.6834121741351,6.82574786431122));
#20499=CARTESIAN_POINT('Origin',(15.8,-13.8493757942074,5.91473145421246));
#20500=CARTESIAN_POINT('Ctrl Pts',(10.0502525316942,-9.36936257048691,5.29266352931554));
#20501=CARTESIAN_POINT('Ctrl Pts',(11.9668350211294,-10.5998888833726,7.11242577089738));
#20502=CARTESIAN_POINT('Ctrl Pts',(13.8834175105647,-11.8304151962582,8.93218801247923));
#20503=CARTESIAN_POINT('Ctrl Pts',(15.8,-13.0609415091439,10.7519502540611));
#20504=CARTESIAN_POINT('Ctrl Pts',(10.0502525316942,-9.19066745032221,5.50090730964532));
#20505=CARTESIAN_POINT('Ctrl Pts',(11.9668350211294,-10.3756997001811,7.33966268788185));
#20506=CARTESIAN_POINT('Ctrl Pts',(13.8834175105647,-11.5602999829831,9.17890569898124));
#20507=CARTESIAN_POINT('Ctrl Pts',(15.8,-12.745332232842,11.0176610772178));
#20508=CARTESIAN_POINT('Ctrl Pts',(10.0502525316942,-8.88494866314842,5.78937538435653));
#20509=CARTESIAN_POINT('Ctrl Pts',(11.9668350211294,-9.99448540715111,7.65168842520523));
#20510=CARTESIAN_POINT('Ctrl Pts',(13.8834175105647,-11.104545703274,9.51341402508183));
#20511=CARTESIAN_POINT('Ctrl Pts',(15.8,-12.2140824472766,11.3757270659305));
#20512=CARTESIAN_POINT('Ctrl Pts',(10.0502525316942,-8.62956238511758,5.83613263565859));
#20513=CARTESIAN_POINT('Ctrl Pts',(11.9668350211294,-9.68562073924798,7.68881403767578));
#20514=CARTESIAN_POINT('Ctrl Pts',(13.8834175105647,-10.7414245752752,9.54180236671465));
#20515=CARTESIAN_POINT('Ctrl Pts',(15.8,-11.7974829294056,11.3944837687318));
#20516=CARTESIAN_POINT('Ctrl Pts',(10.0502525316942,-8.45485763321061,5.80103525788045));
#20517=CARTESIAN_POINT('Ctrl Pts',(11.9668350211294,-9.47972276943763,7.6332697458833));
#20518=CARTESIAN_POINT('Ctrl Pts',(13.8834175105647,-10.5043553237743,9.46570011434025));
#20519=CARTESIAN_POINT('Ctrl Pts',(15.8,-11.5292204600013,11.2979346023431));
#20520=CARTESIAN_POINT('Ctrl Pts',(10.0502525316941,-8.27718317134364,5.77456941285602));
#20521=CARTESIAN_POINT('Ctrl Pts',(11.9668350211294,-9.27115170336996,7.58519358293626));
#20522=CARTESIAN_POINT('Ctrl Pts',(13.8834175105647,-10.2649338319875,9.39609248134292));
#20523=CARTESIAN_POINT('Ctrl Pts',(15.8,-11.2589023640139,11.2067166514232));
#20524=CARTESIAN_POINT('Ctrl Pts',(10.0502525316942,-8.0031076613001,5.75553891274799));
#20525=CARTESIAN_POINT('Ctrl Pts',(11.9668350211295,-8.94781145509674,7.53737545292393));
#20526=CARTESIAN_POINT('Ctrl Pts',(13.8834175105647,-9.89241088219744,9.31923862861202));
#20527=CARTESIAN_POINT('Ctrl Pts',(15.8,-10.8371146759941,11.101075168788));
#20528=CARTESIAN_POINT('Ctrl Pts',(10.0502525316942,-7.76245969237558,5.66702291215723));
#20529=CARTESIAN_POINT('Ctrl Pts',(11.9668350211294,-8.66825218904355,7.4114007810768));
#20530=CARTESIAN_POINT('Ctrl Pts',(13.8834175105647,-9.57397375447812,9.1558448117796));
#20531=CARTESIAN_POINT('Ctrl Pts',(15.8,-10.4797662511461,10.9002226806992));
#20532=CARTESIAN_POINT('Ctrl Pts',(10.0502525316942,-7.54398815168985,5.55269814935977));
#20533=CARTESIAN_POINT('Ctrl Pts',(11.9668350211294,-8.41867077420536,7.25492061800102));
#20534=CARTESIAN_POINT('Ctrl Pts',(13.8834175105647,-9.29328875951756,8.95722517253276));
#20535=CARTESIAN_POINT('Ctrl Pts',(15.8,-10.1679713820331,10.659447641174));
#20536=CARTESIAN_POINT('Ctrl Pts',(10.0502525316942,-7.44587907063767,5.47835809159451));
#20537=CARTESIAN_POINT('Ctrl Pts',(11.9668350211294,-8.30851053998513,7.15753678028296));
#20538=CARTESIAN_POINT('Ctrl Pts',(13.8834175105647,-9.17110734047641,8.83668456248994));
#20539=CARTESIAN_POINT('Ctrl Pts',(15.8,-10.0337388098239,10.5158632511784));
#20540=CARTESIAN_POINT('Ctrl Pts',(10.0502525316942,-7.38503851882133,5.42237201204004));
#20541=CARTESIAN_POINT('Ctrl Pts',(11.9668350211294,-8.24114891510682,7.08526863916361));
#20542=CARTESIAN_POINT('Ctrl Pts',(13.8834175105647,-9.09725931139231,8.74816526628719));
#20543=CARTESIAN_POINT('Ctrl Pts',(15.8,-9.95336970767779,10.4110618934108));
#20544=CARTESIAN_POINT('Ctrl Pts',(15.8,-9.9801646912522,10.4452137610133));
#20545=CARTESIAN_POINT('Ctrl Pts',(15.8,-9.97473811086981,10.4384530463692));
#20546=CARTESIAN_POINT('Ctrl Pts',(15.8,-9.96934533045351,10.4316574943231));
#20547=CARTESIAN_POINT('Ctrl Pts',(15.8,-9.96398633981914,10.4248271146823));
#20548=CARTESIAN_POINT('Ctrl Pts',(15.8,-9.95866113228077,10.4179619142908));
#20549=CARTESIAN_POINT('Ctrl Pts',(15.8,-9.95336970767779,10.4110618934108));
#20550=CARTESIAN_POINT('Origin',(15.8,-11.3437865591856,9.90493637355978));
#20551=CARTESIAN_POINT('Ctrl Pts',(10.0502525316942,-7.2752703501265,7.92891439885425));
#20552=CARTESIAN_POINT('Ctrl Pts',(11.9668350211294,-7.88323296009842,10.0398646795257));
#20553=CARTESIAN_POINT('Ctrl Pts',(13.8834175105647,-8.49119557007034,12.1508149601973));
#20554=CARTESIAN_POINT('Ctrl Pts',(15.8,-9.09915818004226,14.2617652408688));
#20555=CARTESIAN_POINT('Ctrl Pts',(10.0502525316942,-7.04097032456894,8.07174617417205));
#20556=CARTESIAN_POINT('Ctrl Pts',(11.9668350211294,-7.59972129962698,10.186749261509));
#20557=CARTESIAN_POINT('Ctrl Pts',(13.8834175105647,-8.15813578620935,12.3019395333854));
#20558=CARTESIAN_POINT('Ctrl Pts',(15.8,-8.71688676126738,14.4169426207224));
#20559=CARTESIAN_POINT('Ctrl Pts',(10.0502525316942,-6.66138127597024,8.25126590443755));
#20560=CARTESIAN_POINT('Ctrl Pts',(11.9668350211294,-7.14127838379811,10.365200404417));
#20561=CARTESIAN_POINT('Ctrl Pts',(13.8834175105647,-7.62165928459738,12.4788866778492));
#20562=CARTESIAN_POINT('Ctrl Pts',(15.8,-8.10155639242525,14.5928211778286));
#20563=CARTESIAN_POINT('Ctrl Pts',(10.0502525316942,-6.42930419296208,8.22079862024225));
#20564=CARTESIAN_POINT('Ctrl Pts',(11.9668350211294,-6.86580395314968,10.3118069242151));
#20565=CARTESIAN_POINT('Ctrl Pts',(13.8834175105647,-7.3023483954802,12.4027801127282));
#20566=CARTESIAN_POINT('Ctrl Pts',(15.8,-7.73884815566781,14.493788416701));
#20567=CARTESIAN_POINT('Ctrl Pts',(10.0502525316942,-6.30697938690416,8.16221173215364));
#20568=CARTESIAN_POINT('Ctrl Pts',(11.9668350211294,-6.72434771418857,10.2323186327506));
#20569=CARTESIAN_POINT('Ctrl Pts',(13.8834175105647,-7.14137150628509,12.3026176380752));
#20570=CARTESIAN_POINT('Ctrl Pts',(15.8,-7.5587398335695,14.3727245386721));
#20571=CARTESIAN_POINT('Ctrl Pts',(10.0502525316942,-6.22815403351084,8.12000643506485));
#20572=CARTESIAN_POINT('Ctrl Pts',(11.9668350211294,-6.63375833246635,10.1755454476056));
#20573=CARTESIAN_POINT('Ctrl Pts',(13.8834175105647,-7.03916552489902,12.2311493413123));
#20574=CARTESIAN_POINT('Ctrl Pts',(15.8,-7.44476982385453,14.2866883538531));
#20575=CARTESIAN_POINT('Ctrl Pts',(10.0502525316942,-6.08789997184504,8.04942040067478));
#20576=CARTESIAN_POINT('Ctrl Pts',(11.9668350211294,-6.47376321403759,10.0785454407991));
#20577=CARTESIAN_POINT('Ctrl Pts',(13.8834175105647,-6.85942462405723,12.1078515605739));
#20578=CARTESIAN_POINT('Ctrl Pts',(15.8,-7.24528786624977,14.1369766006982));
#20579=CARTESIAN_POINT('Ctrl Pts',(10.0502525316942,-5.83267830770085,7.94713925110583));
#20580=CARTESIAN_POINT('Ctrl Pts',(11.9668350211294,-6.18048893841474,9.93371906448112));
#20581=CARTESIAN_POINT('Ctrl Pts',(13.8834175105647,-6.52817426230451,11.920292369998));
#20582=CARTESIAN_POINT('Ctrl Pts',(15.8,-6.87598489301839,13.9068721833733));
#20583=CARTESIAN_POINT('Ctrl Pts',(10.0502525316942,-5.63138575926578,7.78832910259187));
#20584=CARTESIAN_POINT('Ctrl Pts',(11.9668350211294,-5.95382183425814,9.7272251121909));
#20585=CARTESIAN_POINT('Ctrl Pts',(13.8834175105647,-6.27616146093385,11.6661698490829));
#20586=CARTESIAN_POINT('Ctrl Pts',(15.8,-6.59859753592621,13.605065858682));
#20587=CARTESIAN_POINT('Ctrl Pts',(10.0502525316942,-5.45884429554414,7.61219406851115));
#20588=CARTESIAN_POINT('Ctrl Pts',(11.9668350211294,-5.76468621283309,9.50140467053763));
#20589=CARTESIAN_POINT('Ctrl Pts',(13.8834175105647,-6.07045912241827,11.3906602079427));
#20590=CARTESIAN_POINT('Ctrl Pts',(15.8,-6.37630103970722,13.2798708099692));
#20591=CARTESIAN_POINT('Ctrl Pts',(10.0502525316942,-5.38854605810145,7.51113133249701));
#20592=CARTESIAN_POINT('Ctrl Pts',(11.9668350211294,-5.69007333772413,9.37468648227302));
#20593=CARTESIAN_POINT('Ctrl Pts',(13.8834175105647,-5.99154494312677,11.238220929081));
#20594=CARTESIAN_POINT('Ctrl Pts',(15.8,-6.29307222274945,13.101776078857));
#20595=CARTESIAN_POINT('Ctrl Pts',(10.0502525316942,-5.34798390487229,7.43908464225652));
#20596=CARTESIAN_POINT('Ctrl Pts',(11.9668350211294,-5.64832995825767,9.28514597692092));
#20597=CARTESIAN_POINT('Ctrl Pts',(13.8834175105647,-5.94867601164304,11.1312073115853));
#20598=CARTESIAN_POINT('Ctrl Pts',(15.8,-6.24902206502841,12.9772686462497));
#20599=CARTESIAN_POINT('Ctrl Pts',(15.8,-6.26395210128206,13.0180291077652));
#20600=CARTESIAN_POINT('Ctrl Pts',(15.8,-6.26088029236732,13.0099223804886));
#20601=CARTESIAN_POINT('Ctrl Pts',(15.8,-6.25785139447984,13.0017929656379));
#20602=CARTESIAN_POINT('Ctrl Pts',(15.8,-6.25486539490331,12.993640869393));
#20603=CARTESIAN_POINT('Ctrl Pts',(15.8,-6.25192228516409,12.985466096197));
#20604=CARTESIAN_POINT('Ctrl Pts',(15.8,-6.24902206502841,12.9772686462497));
#20605=CARTESIAN_POINT('Origin',(15.8,-7.7277884589423,12.9255771089134));
#20606=CARTESIAN_POINT('Ctrl Pts',(10.0502525316942,-4.46902397810655,9.78902788303806));
#20607=CARTESIAN_POINT('Ctrl Pts',(11.9668350211294,-4.39491126897609,11.9845316814717));
#20608=CARTESIAN_POINT('Ctrl Pts',(13.8834175105647,-4.32079855984564,14.1800354799052));
#20609=CARTESIAN_POINT('Ctrl Pts',(15.8,-4.24668585071518,16.3755392783388));
#20610=CARTESIAN_POINT('Ctrl Pts',(10.0502525316942,-4.20205396612196,9.8524662840083));
#20611=CARTESIAN_POINT('Ctrl Pts',(11.9668350211294,-4.07988582479457,12.036617299121));
#20612=CARTESIAN_POINT('Ctrl Pts',(13.8834175105647,-3.95733982070598,14.2208423566523));
#20613=CARTESIAN_POINT('Ctrl Pts',(15.8,-3.83517167937858,16.404993371765));
#20614=CARTESIAN_POINT('Ctrl Pts',(10.0502525316942,-3.78556561092159,9.90590216992165));
#20615=CARTESIAN_POINT('Ctrl Pts',(11.9668350211295,-3.58873319698333,12.0646697130184));
#20616=CARTESIAN_POINT('Ctrl Pts',(13.8834175105647,-3.39243568541408,14.2233509855394));
#20617=CARTESIAN_POINT('Ctrl Pts',(15.8,-3.19560327147581,16.3821185286362));
#20618=CARTESIAN_POINT('Ctrl Pts',(10.0502525316942,-3.57425782911967,9.80521299123422));
#20619=CARTESIAN_POINT('Ctrl Pts',(11.9668350211295,-3.34323666910062,11.9287659082934));
#20620=CARTESIAN_POINT('Ctrl Pts',(13.8834175105647,-3.11226431322854,14.0522999619539));
#20621=CARTESIAN_POINT('Ctrl Pts',(15.8,-2.8812431532095,16.1758528790131));
#20622=CARTESIAN_POINT('Ctrl Pts',(10.0502525316942,-3.47602249721152,9.71169428155716));
#20623=CARTESIAN_POINT('Ctrl Pts',(11.9668350211295,-3.23326515211327,11.8094568448422));
#20624=CARTESIAN_POINT('Ctrl Pts',(13.8834175105647,-2.99011502771357,13.9072965714997));
#20625=CARTESIAN_POINT('Ctrl Pts',(15.8,-2.74735768261532,16.0050591347847));
#20626=CARTESIAN_POINT('Ctrl Pts',(10.0502525316942,-3.414097226746,9.64719632995103));
#20627=CARTESIAN_POINT('Ctrl Pts',(11.9668350211295,-3.16465335082918,11.7274687236956));
#20628=CARTESIAN_POINT('Ctrl Pts',(13.8834175105647,-2.91499625447087,13.8077428217682));
#20629=CARTESIAN_POINT('Ctrl Pts',(15.8,-2.66555237855405,15.8880152155128));
#20630=CARTESIAN_POINT('Ctrl Pts',(10.0502525316942,-3.30251999207182,9.53672408685997));
#20631=CARTESIAN_POINT('Ctrl Pts',(11.9668350211294,-3.04246362184766,11.58577497799));
#20632=CARTESIAN_POINT('Ctrl Pts',(13.8834175105647,-2.7821533789288,13.6349367240444));
#20633=CARTESIAN_POINT('Ctrl Pts',(15.8,-2.52209700870464,15.6839876151744));
#20634=CARTESIAN_POINT('Ctrl Pts',(10.0502525316942,-3.09139659750779,9.36058107581316));
#20635=CARTESIAN_POINT('Ctrl Pts',(11.9668350211295,-2.80829724126978,11.357410148179));
#20636=CARTESIAN_POINT('Ctrl Pts',(13.8834175105647,-2.52507603204707,13.3541948572957));
#20637=CARTESIAN_POINT('Ctrl Pts',(15.8,-2.24197667580906,15.3510239296616));
#20638=CARTESIAN_POINT('Ctrl Pts',(10.0502525316942,-2.94903314862294,9.14733948977135));
#20639=CARTESIAN_POINT('Ctrl Pts',(11.9668350211294,-2.65653626154119,11.0909774008914));
#20640=CARTESIAN_POINT('Ctrl Pts',(13.8834175105647,-2.36392896441619,13.0346322911662));
#20641=CARTESIAN_POINT('Ctrl Pts',(15.8,-2.07143207733444,14.9782702022863));
#20642=CARTESIAN_POINT('Ctrl Pts',(10.0502525316942,-2.83936642791009,8.92650608260145));
#20643=CARTESIAN_POINT('Ctrl Pts',(11.9668350211294,-2.54644119432445,10.8177624863471));
#20644=CARTESIAN_POINT('Ctrl Pts',(13.8834175105648,-2.25343349088951,12.7090406610097));
#20645=CARTESIAN_POINT('Ctrl Pts',(15.8,-1.96050825730386,14.6002970647553));
#20646=CARTESIAN_POINT('Ctrl Pts',(10.0502525316942,-2.80374461319022,8.80866270544546));
#20647=CARTESIAN_POINT('Ctrl Pts',(11.9668350211294,-2.51464388608039,10.6741860277864));
#20648=CARTESIAN_POINT('Ctrl Pts',(13.8834175105647,-2.22549660720977,12.5396724561545));
#20649=CARTESIAN_POINT('Ctrl Pts',(15.8,-1.93639588009993,14.4051957784954));
#20650=CARTESIAN_POINT('Ctrl Pts',(10.0502525316942,-2.78743136471945,8.7276078365385));
#20651=CARTESIAN_POINT('Ctrl Pts',(11.9668350211294,-2.50261311086535,10.5761285330411));
#20652=CARTESIAN_POINT('Ctrl Pts',(13.8834175105647,-2.21779485701124,12.4246492295437));
#20653=CARTESIAN_POINT('Ctrl Pts',(15.8,-1.93297660315714,14.2731699260464));
#20654=CARTESIAN_POINT('Ctrl Pts',(15.8,-1.93458023611785,14.3165490635069));
#20655=CARTESIAN_POINT('Ctrl Pts',(15.8,-1.93416388872989,14.3078898665466));
#20656=CARTESIAN_POINT('Ctrl Pts',(15.8,-1.93379536300002,14.2992223526576));
#20657=CARTESIAN_POINT('Ctrl Pts',(15.8,-1.93347464492456,14.2905465237881));
#20658=CARTESIAN_POINT('Ctrl Pts',(15.8,-1.93320172507161,14.2818623815451));
#20659=CARTESIAN_POINT('Ctrl Pts',(15.8,-1.93297660315714,14.2731699260464));
#20660=CARTESIAN_POINT('Origin',(15.8,-3.35534058166953,14.6809722990553));
#20661=CARTESIAN_POINT('Ctrl Pts',(10.0502525316942,-1.22531840158854,10.6909231138624));
#20662=CARTESIAN_POINT('Ctrl Pts',(11.9668350211294,-0.47638504169901,12.7560692212929));
#20663=CARTESIAN_POINT('Ctrl Pts',(13.8834175105647,0.272548318190524,14.8212153287235));
#20664=CARTESIAN_POINT('Ctrl Pts',(15.8,1.02148167808006,16.886361436154));
#20665=CARTESIAN_POINT('Ctrl Pts',(10.0502525316942,-0.951811288039438,
10.6687583477967));
#20666=CARTESIAN_POINT('Ctrl Pts',(11.9668350211294,-0.160771418505768,
12.7082628707158));
#20667=CARTESIAN_POINT('Ctrl Pts',(13.8834175105647,0.630916858166453,14.7477045483503));
#20668=CARTESIAN_POINT('Ctrl Pts',(15.8,1.42195672770012,16.7872090712694));
#20669=CARTESIAN_POINT('Ctrl Pts',(10.0502525316942,-0.538737970192933,
10.5909841198542));
#20670=CARTESIAN_POINT('Ctrl Pts',(11.9668350211295,0.315735593698357,12.5832583421986));
#20671=CARTESIAN_POINT('Ctrl Pts',(13.8834175105647,1.16942659814005,14.5756107736058));
#20672=CARTESIAN_POINT('Ctrl Pts',(15.8,2.02390016203134,16.5678849959503));
#20673=CARTESIAN_POINT('Ctrl Pts',(10.0502525316942,-0.350797420983486,
10.4118557126012));
#20674=CARTESIAN_POINT('Ctrl Pts',(11.9668350211295,0.527317792292715,12.3552036734465));
#20675=CARTESIAN_POINT('Ctrl Pts',(13.8834175105647,1.40583184426593,14.2985259967778));
#20676=CARTESIAN_POINT('Ctrl Pts',(15.8,2.28394705754214,16.2418739576232));
#20677=CARTESIAN_POINT('Ctrl Pts',(10.0502525316942,-0.276502431596344,
10.2498870013208));
#20678=CARTESIAN_POINT('Ctrl Pts',(11.9668350211295,0.60340579421488,12.1559807242605));
#20679=CARTESIAN_POINT('Ctrl Pts',(13.8834175105647,1.48361038150706,14.0620012424206));
#20680=CARTESIAN_POINT('Ctrl Pts',(15.8,2.36351860731828,15.9680949653604));
#20681=CARTESIAN_POINT('Ctrl Pts',(10.0502525316942,-0.193479460458703,
10.0905890686414));
#20682=CARTESIAN_POINT('Ctrl Pts',(11.9668350211294,0.687106219194375,11.9589846875421));
#20683=CARTESIAN_POINT('Ctrl Pts',(13.8834175105647,1.56802487912709,13.8273908205778));
#20684=CARTESIAN_POINT('Ctrl Pts',(15.8,2.44861055878017,15.6957864394785));
#20685=CARTESIAN_POINT('Ctrl Pts',(10.0502525316942,-0.0477779613143534,
9.85767148446325));
#20686=CARTESIAN_POINT('Ctrl Pts',(11.9668350211294,0.838475123107829,11.6692901486065));
#20687=CARTESIAN_POINT('Ctrl Pts',(13.8834175105647,1.72481200902093,13.4808398643785));
#20688=CARTESIAN_POINT('Ctrl Pts',(15.8,2.61106509344311,15.2924585285217));
#20689=CARTESIAN_POINT('Ctrl Pts',(10.0502525316942,0.0220599042734169,
9.61095465953459));
#20690=CARTESIAN_POINT('Ctrl Pts',(11.9668350211294,0.900879773662288,11.3690757684926));
#20691=CARTESIAN_POINT('Ctrl Pts',(13.8834175105647,1.77979551853006,13.1271782591657));
#20692=CARTESIAN_POINT('Ctrl Pts',(15.8,2.65861538791893,14.8852993681237));
#20693=CARTESIAN_POINT('Ctrl Pts',(10.0502525316942,0.0579833517275568,
9.36700900338232));
#20694=CARTESIAN_POINT('Ctrl Pts',(11.9668350211294,0.920984711114088,11.07518337287));
#20695=CARTESIAN_POINT('Ctrl Pts',(13.8834175105647,1.78409102238058,12.7833535968728));
#20696=CARTESIAN_POINT('Ctrl Pts',(15.8,2.64709238176711,14.4915279663605));
#20697=CARTESIAN_POINT('Ctrl Pts',(10.0502525316942,0.0555068892974573,
9.243940799223));
#20698=CARTESIAN_POINT('Ctrl Pts',(11.9668350211294,0.906948929192825,10.9288207869826));
#20699=CARTESIAN_POINT('Ctrl Pts',(13.8834175105647,1.75838634306183,12.6136545606744));
#20700=CARTESIAN_POINT('Ctrl Pts',(15.8,2.6098283829572,14.298534548434));
#20701=CARTESIAN_POINT('Ctrl Pts',(10.0502525316942,0.0459743785884363,
9.16181196696065));
#20702=CARTESIAN_POINT('Ctrl Pts',(11.9668350211294,0.888076944549314,10.8318459401268));
#20703=CARTESIAN_POINT('Ctrl Pts',(13.8834175105647,1.73017951051019,12.501879913293));
#20704=CARTESIAN_POINT('Ctrl Pts',(15.8,2.57228207647107,14.1719138864591));
#20705=CARTESIAN_POINT('Ctrl Pts',(15.8,2.58416182157067,14.2136654476498));
#20706=CARTESIAN_POINT('Ctrl Pts',(15.8,2.58188195244865,14.2053014035364));
#20707=CARTESIAN_POINT('Ctrl Pts',(15.8,2.57955403215479,14.1969442272588));
#20708=CARTESIAN_POINT('Ctrl Pts',(15.8,2.57717807460939,14.1885939163425));
#20709=CARTESIAN_POINT('Ctrl Pts',(15.8,2.57475408927931,14.1802504694012));
#20710=CARTESIAN_POINT('Ctrl Pts',(15.8,2.57228207647107,14.1719138864591));
#20711=CARTESIAN_POINT('Origin',(15.8,1.34555140976955,14.999291632217));
#20712=CARTESIAN_POINT('Ctrl Pts',(10.0502525316942,2.13832987737225,10.5463163022605));
#20713=CARTESIAN_POINT('Ctrl Pts',(11.9668350211294,3.48877307262933,12.2789538289737));
#20714=CARTESIAN_POINT('Ctrl Pts',(13.8834175105647,4.8392162678864,14.0115913556869));
#20715=CARTESIAN_POINT('Ctrl Pts',(15.8,6.18965946314348,15.7442288824001));
#20716=CARTESIAN_POINT('Ctrl Pts',(10.0502525316942,2.39160131057558,10.4407180108925));
#20717=CARTESIAN_POINT('Ctrl Pts',(11.9668350211294,3.77416649083142,12.1359573145141));
#20718=CARTESIAN_POINT('Ctrl Pts',(13.8834175105647,5.15732892266062,13.8309364798931));
#20719=CARTESIAN_POINT('Ctrl Pts',(15.8,6.53989410291645,15.5261757835147));
#20720=CARTESIAN_POINT('Ctrl Pts',(10.0502525316942,2.7604211119455,10.2391038402362));
#20721=CARTESIAN_POINT('Ctrl Pts',(11.9668350211294,4.18872035504581,11.8698223691572));
#20722=CARTESIAN_POINT('Ctrl Pts',(13.8834175105647,5.61629814839674,13.5008577836237));
#20723=CARTESIAN_POINT('Ctrl Pts',(15.8,7.04459739149705,15.1315763125447));
#20724=CARTESIAN_POINT('Ctrl Pts',(10.0502525316942,2.88380634898392,10.0106660065973));
#20725=CARTESIAN_POINT('Ctrl Pts',(11.9668350211294,4.31947109051328,11.5875472242667));
#20726=CARTESIAN_POINT('Ctrl Pts',(13.8834175105647,5.75550424110768,13.1642822866716));
#20727=CARTESIAN_POINT('Ctrl Pts',(15.8,7.19116898263704,14.7411635043409));
#20728=CARTESIAN_POINT('Ctrl Pts',(10.0502525316942,2.90441220847246,9.83366631411431));
#20729=CARTESIAN_POINT('Ctrl Pts',(11.9668350211294,4.33027001363173,11.3745625747195));
#20730=CARTESIAN_POINT('Ctrl Pts',(13.8834175105647,5.75638324902558,12.9152995332973));
#20731=CARTESIAN_POINT('Ctrl Pts',(15.8,7.18224105418486,14.4561957939025));
#20732=CARTESIAN_POINT('Ctrl Pts',(10.0502525316941,2.93414649567711,9.65650945139357));
#20733=CARTESIAN_POINT('Ctrl Pts',(11.9668350211294,4.34899924292338,11.1613433397504));
#20734=CARTESIAN_POINT('Ctrl Pts',(13.8834175105647,5.76416819477547,12.6660861533134));
#20735=CARTESIAN_POINT('Ctrl Pts',(15.8,7.17902094202174,14.1709200416702));
#20736=CARTESIAN_POINT('Ctrl Pts',(10.0502525316942,3.00074150798572,9.38996734645583));
#20737=CARTESIAN_POINT('Ctrl Pts',(11.9668350211294,4.40343923355921,10.8390518176275));
#20738=CARTESIAN_POINT('Ctrl Pts',(13.8834175105647,5.8061924752444,12.2880463890102));
#20739=CARTESIAN_POINT('Ctrl Pts',(15.8,7.20889020081789,13.7371308601818));
#20740=CARTESIAN_POINT('Ctrl Pts',(10.0502525316942,2.99092345166592,9.13374448664766));
#20741=CARTESIAN_POINT('Ctrl Pts',(11.9668350211294,4.37002011593521,10.5342467491227));
#20742=CARTESIAN_POINT('Ctrl Pts',(13.8834175105647,5.74920012742636,11.9347028120052));
#20743=CARTESIAN_POINT('Ctrl Pts',(15.8,7.12829679169565,13.3352050744803));
#20744=CARTESIAN_POINT('Ctrl Pts',(10.0502525316942,2.94970615383951,8.89063737063806));
#20745=CARTESIAN_POINT('Ctrl Pts',(11.9668350211294,4.29832412978306,10.2485256494886));
#20746=CARTESIAN_POINT('Ctrl Pts',(13.8834175105647,5.64703889510258,11.6063785007713));
#20747=CARTESIAN_POINT('Ctrl Pts',(15.8,6.99565687104613,12.9642667796218));
#20748=CARTESIAN_POINT('Ctrl Pts',(10.0502525316942,2.90932499072146,8.77435756124986));
#20749=CARTESIAN_POINT('Ctrl Pts',(11.9668350211294,4.23975104071156,10.113663592731));
#20750=CARTESIAN_POINT('Ctrl Pts',(13.8834175105647,5.57015841015681,11.4529271015425));
#20751=CARTESIAN_POINT('Ctrl Pts',(15.8,6.90058446014691,12.7922331330237));
#20752=CARTESIAN_POINT('Ctrl Pts',(10.0502525316942,2.87487982939776,8.69919410795919));
#20753=CARTESIAN_POINT('Ctrl Pts',(11.9668350211294,4.19183584103558,10.0272667966845));
#20754=CARTESIAN_POINT('Ctrl Pts',(13.8834175105647,5.5087918526734,11.3553394854098));
#20755=CARTESIAN_POINT('Ctrl Pts',(15.8,6.82574786431122,12.6834121741351));
#20756=CARTESIAN_POINT('Ctrl Pts',(15.8,6.84994811524973,12.7194492253464));
#20757=CARTESIAN_POINT('Ctrl Pts',(15.8,6.84519519909218,12.7121990649934));
#20758=CARTESIAN_POINT('Ctrl Pts',(15.8,6.84039870583253,12.7049702849691));
#20759=CARTESIAN_POINT('Ctrl Pts',(15.8,6.83555864794507,12.6977628786185));
#20760=CARTESIAN_POINT('Ctrl Pts',(15.8,6.83067503400497,12.6905768416977));
#20761=CARTESIAN_POINT('Ctrl Pts',(15.8,6.82574786431122,12.6834121741351));
#20762=CARTESIAN_POINT('Origin',(15.8,5.91473145421246,13.8493757942074));
#20763=CARTESIAN_POINT('Ctrl Pts',(10.0502525316942,5.29266352931554,9.36936257048691));
#20764=CARTESIAN_POINT('Ctrl Pts',(11.9668350211294,7.11242577089738,10.5998888833726));
#20765=CARTESIAN_POINT('Ctrl Pts',(13.8834175105647,8.93218801247923,11.8304151962582));
#20766=CARTESIAN_POINT('Ctrl Pts',(15.8,10.7519502540611,13.0609415091439));
#20767=CARTESIAN_POINT('Ctrl Pts',(10.0502525316942,5.50090730964532,9.19066745032222));
#20768=CARTESIAN_POINT('Ctrl Pts',(11.9668350211294,7.33966268788185,10.3756997001811));
#20769=CARTESIAN_POINT('Ctrl Pts',(13.8834175105647,9.17890569898124,11.5602999829831));
#20770=CARTESIAN_POINT('Ctrl Pts',(15.8,11.0176610772178,12.745332232842));
#20771=CARTESIAN_POINT('Ctrl Pts',(10.0502525316942,5.78937538435654,8.88494866314842));
#20772=CARTESIAN_POINT('Ctrl Pts',(11.9668350211294,7.65168842520523,9.99448540715111));
#20773=CARTESIAN_POINT('Ctrl Pts',(13.8834175105647,9.51341402508183,11.104545703274));
#20774=CARTESIAN_POINT('Ctrl Pts',(15.8,11.3757270659305,12.2140824472767));
#20775=CARTESIAN_POINT('Ctrl Pts',(10.0502525316942,5.83613263565858,8.62956238511758));
#20776=CARTESIAN_POINT('Ctrl Pts',(11.9668350211294,7.68881403767577,9.68562073924798));
#20777=CARTESIAN_POINT('Ctrl Pts',(13.8834175105647,9.54180236671465,10.7414245752752));
#20778=CARTESIAN_POINT('Ctrl Pts',(15.8,11.3944837687318,11.7974829294056));
#20779=CARTESIAN_POINT('Ctrl Pts',(10.0502525316942,5.80103525788045,8.45485763321062));
#20780=CARTESIAN_POINT('Ctrl Pts',(11.9668350211294,7.63326974588329,9.47972276943764));
#20781=CARTESIAN_POINT('Ctrl Pts',(13.8834175105647,9.46570011434026,10.5043553237743));
#20782=CARTESIAN_POINT('Ctrl Pts',(15.8,11.2979346023431,11.5292204600013));
#20783=CARTESIAN_POINT('Ctrl Pts',(10.0502525316941,5.77456941285602,8.27718317134364));
#20784=CARTESIAN_POINT('Ctrl Pts',(11.9668350211294,7.58519358293626,9.27115170336997));
#20785=CARTESIAN_POINT('Ctrl Pts',(13.8834175105647,9.39609248134292,10.2649338319875));
#20786=CARTESIAN_POINT('Ctrl Pts',(15.8,11.2067166514232,11.2589023640138));
#20787=CARTESIAN_POINT('Ctrl Pts',(10.0502525316942,5.75553891274797,8.00310766130011));
#20788=CARTESIAN_POINT('Ctrl Pts',(11.9668350211295,7.53737545292391,8.94781145509674));
#20789=CARTESIAN_POINT('Ctrl Pts',(13.8834175105647,9.31923862861205,9.89241088219743));
#20790=CARTESIAN_POINT('Ctrl Pts',(15.8,11.101075168788,10.8371146759941));
#20791=CARTESIAN_POINT('Ctrl Pts',(10.0502525316942,5.66702291215725,7.76245969237559));
#20792=CARTESIAN_POINT('Ctrl Pts',(11.9668350211294,7.41140078107682,8.66825218904356));
#20793=CARTESIAN_POINT('Ctrl Pts',(13.8834175105647,9.15584481177958,9.57397375447815));
#20794=CARTESIAN_POINT('Ctrl Pts',(15.8,10.9002226806991,10.4797662511461));
#20795=CARTESIAN_POINT('Ctrl Pts',(10.0502525316942,5.55269814935977,7.54398815168985));
#20796=CARTESIAN_POINT('Ctrl Pts',(11.9668350211294,7.25492061800102,8.41867077420536));
#20797=CARTESIAN_POINT('Ctrl Pts',(13.8834175105647,8.95722517253276,9.29328875951754));
#20798=CARTESIAN_POINT('Ctrl Pts',(15.8,10.659447641174,10.167971382033));
#20799=CARTESIAN_POINT('Ctrl Pts',(10.0502525316942,5.47835809159451,7.44587907063767));
#20800=CARTESIAN_POINT('Ctrl Pts',(11.9668350211294,7.15753678028296,8.30851053998513));
#20801=CARTESIAN_POINT('Ctrl Pts',(13.8834175105647,8.83668456248994,9.17110734047641));
#20802=CARTESIAN_POINT('Ctrl Pts',(15.8,10.5158632511784,10.0337388098239));
#20803=CARTESIAN_POINT('Ctrl Pts',(10.0502525316942,5.42237201204004,7.38503851882133));
#20804=CARTESIAN_POINT('Ctrl Pts',(11.9668350211294,7.08526863916361,8.24114891510682));
#20805=CARTESIAN_POINT('Ctrl Pts',(13.8834175105647,8.74816526628719,9.09725931139231));
#20806=CARTESIAN_POINT('Ctrl Pts',(15.8,10.4110618934108,9.9533697076778));
#20807=CARTESIAN_POINT('Ctrl Pts',(15.8,10.4452137610132,9.98016469125221));
#20808=CARTESIAN_POINT('Ctrl Pts',(15.8,10.4384530463692,9.97473811086981));
#20809=CARTESIAN_POINT('Ctrl Pts',(15.8,10.4316574943231,9.96934533045351));
#20810=CARTESIAN_POINT('Ctrl Pts',(15.8,10.4248271146823,9.96398633981914));
#20811=CARTESIAN_POINT('Ctrl Pts',(15.8,10.4179619142908,9.95866113228077));
#20812=CARTESIAN_POINT('Ctrl Pts',(15.8,10.4110618934108,9.9533697076778));
#20813=CARTESIAN_POINT('Origin',(15.8,9.90493637355978,11.3437865591856));
#20814=CARTESIAN_POINT('Ctrl Pts',(10.0502525316942,7.92891439885425,7.2752703501265));
#20815=CARTESIAN_POINT('Ctrl Pts',(11.9668350211294,10.0398646795257,7.88323296009842));
#20816=CARTESIAN_POINT('Ctrl Pts',(13.8834175105647,12.1508149601973,8.49119557007034));
#20817=CARTESIAN_POINT('Ctrl Pts',(15.8,14.2617652408688,9.09915818004226));
#20818=CARTESIAN_POINT('Ctrl Pts',(10.0502525316942,8.07174617417204,7.04097032456894));
#20819=CARTESIAN_POINT('Ctrl Pts',(11.9668350211294,10.186749261509,7.59972129962697));
#20820=CARTESIAN_POINT('Ctrl Pts',(13.8834175105647,12.3019395333854,8.15813578620935));
#20821=CARTESIAN_POINT('Ctrl Pts',(15.8,14.4169426207224,8.71688676126738));
#20822=CARTESIAN_POINT('Ctrl Pts',(10.0502525316942,8.25126590443757,6.66138127597024));
#20823=CARTESIAN_POINT('Ctrl Pts',(11.9668350211294,10.365200404417,7.14127838379811));
#20824=CARTESIAN_POINT('Ctrl Pts',(13.8834175105647,12.4788866778492,7.62165928459738));
#20825=CARTESIAN_POINT('Ctrl Pts',(15.8,14.5928211778287,8.10155639242526));
#20826=CARTESIAN_POINT('Ctrl Pts',(10.0502525316942,8.22079862024226,6.42930419296207));
#20827=CARTESIAN_POINT('Ctrl Pts',(11.9668350211294,10.3118069242151,6.86580395314968));
#20828=CARTESIAN_POINT('Ctrl Pts',(13.8834175105647,12.4027801127282,7.30234839548021));
#20829=CARTESIAN_POINT('Ctrl Pts',(15.8,14.493788416701,7.73884815566781));
#20830=CARTESIAN_POINT('Ctrl Pts',(10.0502525316942,8.16221173215365,6.30697938690416));
#20831=CARTESIAN_POINT('Ctrl Pts',(11.9668350211294,10.2323186327506,6.72434771418857));
#20832=CARTESIAN_POINT('Ctrl Pts',(13.8834175105647,12.3026176380752,7.1413715062851));
#20833=CARTESIAN_POINT('Ctrl Pts',(15.8,14.3727245386721,7.55873983356951));
#20834=CARTESIAN_POINT('Ctrl Pts',(10.0502525316942,8.12000643506487,6.22815403351084));
#20835=CARTESIAN_POINT('Ctrl Pts',(11.9668350211294,10.1755454476056,6.63375833246636));
#20836=CARTESIAN_POINT('Ctrl Pts',(13.8834175105647,12.2311493413123,7.03916552489903));
#20837=CARTESIAN_POINT('Ctrl Pts',(15.8,14.2866883538531,7.44476982385454));
#20838=CARTESIAN_POINT('Ctrl Pts',(10.0502525316942,8.04942040067478,6.08789997184504));
#20839=CARTESIAN_POINT('Ctrl Pts',(11.9668350211294,10.0785454407991,6.47376321403759));
#20840=CARTESIAN_POINT('Ctrl Pts',(13.8834175105647,12.1078515605739,6.85942462405723));
#20841=CARTESIAN_POINT('Ctrl Pts',(15.8,14.1369766006982,7.24528786624978));
#20842=CARTESIAN_POINT('Ctrl Pts',(10.0502525316942,7.94713925110584,5.83267830770086));
#20843=CARTESIAN_POINT('Ctrl Pts',(11.9668350211294,9.93371906448114,6.18048893841474));
#20844=CARTESIAN_POINT('Ctrl Pts',(13.8834175105647,11.920292369998,6.52817426230452));
#20845=CARTESIAN_POINT('Ctrl Pts',(15.8,13.9068721833733,6.8759848930184));
#20846=CARTESIAN_POINT('Ctrl Pts',(10.0502525316942,7.78832910259186,5.63138575926578));
#20847=CARTESIAN_POINT('Ctrl Pts',(11.9668350211294,9.72722511219089,5.95382183425815));
#20848=CARTESIAN_POINT('Ctrl Pts',(13.8834175105647,11.6661698490829,6.27616146093386));
#20849=CARTESIAN_POINT('Ctrl Pts',(15.8,13.605065858682,6.59859753592622));
#20850=CARTESIAN_POINT('Ctrl Pts',(10.0502525316942,7.61219406851114,5.45884429554414));
#20851=CARTESIAN_POINT('Ctrl Pts',(11.9668350211294,9.50140467053761,5.76468621283309));
#20852=CARTESIAN_POINT('Ctrl Pts',(13.8834175105648,11.3906602079427,6.07045912241829));
#20853=CARTESIAN_POINT('Ctrl Pts',(15.8,13.2798708099692,6.37630103970724));
#20854=CARTESIAN_POINT('Ctrl Pts',(10.0502525316942,7.51113133249701,5.38854605810145));
#20855=CARTESIAN_POINT('Ctrl Pts',(11.9668350211294,9.37468648227302,5.69007333772413));
#20856=CARTESIAN_POINT('Ctrl Pts',(13.8834175105647,11.238220929081,5.99154494312677));
#20857=CARTESIAN_POINT('Ctrl Pts',(15.8,13.101776078857,6.29307222274946));
#20858=CARTESIAN_POINT('Ctrl Pts',(10.0502525316942,7.43908464225652,5.34798390487229));
#20859=CARTESIAN_POINT('Ctrl Pts',(11.9668350211294,9.28514597692092,5.64832995825767));
#20860=CARTESIAN_POINT('Ctrl Pts',(13.8834175105647,11.1312073115853,5.94867601164304));
#20861=CARTESIAN_POINT('Ctrl Pts',(15.8,12.9772686462497,6.24902206502841));
#20862=CARTESIAN_POINT('Ctrl Pts',(15.8,13.0180291077652,6.26395210128207));
#20863=CARTESIAN_POINT('Ctrl Pts',(15.8,13.0099223804886,6.26088029236733));
#20864=CARTESIAN_POINT('Ctrl Pts',(15.8,13.0017929656379,6.25785139447984));
#20865=CARTESIAN_POINT('Ctrl Pts',(15.8,12.993640869393,6.25486539490331));
#20866=CARTESIAN_POINT('Ctrl Pts',(15.8,12.985466096197,6.25192228516409));
#20867=CARTESIAN_POINT('Ctrl Pts',(15.8,12.9772686462497,6.24902206502841));
#20868=CARTESIAN_POINT('Origin',(15.8,12.9255771089134,7.7277884589423));
#20869=CARTESIAN_POINT('Ctrl Pts',(10.0502525316942,9.78902788303806,4.46902397810655));
#20870=CARTESIAN_POINT('Ctrl Pts',(11.9668350211294,11.9845316814717,4.39491126897609));
#20871=CARTESIAN_POINT('Ctrl Pts',(13.8834175105647,14.1800354799052,4.32079855984564));
#20872=CARTESIAN_POINT('Ctrl Pts',(15.8,16.3755392783388,4.24668585071518));
#20873=CARTESIAN_POINT('Ctrl Pts',(10.0502525316942,9.8524662840083,4.20205396612197));
#20874=CARTESIAN_POINT('Ctrl Pts',(11.9668350211294,12.036617299121,4.07988582479457));
#20875=CARTESIAN_POINT('Ctrl Pts',(13.8834175105647,14.2208423566523,3.95733982070599));
#20876=CARTESIAN_POINT('Ctrl Pts',(15.8,16.404993371765,3.83517167937859));
#20877=CARTESIAN_POINT('Ctrl Pts',(10.0502525316942,9.90590216992165,3.7855656109216));
#20878=CARTESIAN_POINT('Ctrl Pts',(11.9668350211295,12.0646697130184,3.58873319698334));
#20879=CARTESIAN_POINT('Ctrl Pts',(13.8834175105648,14.2233509855394,3.39243568541407));
#20880=CARTESIAN_POINT('Ctrl Pts',(15.8,16.3821185286362,3.19560327147581));
#20881=CARTESIAN_POINT('Ctrl Pts',(10.0502525316942,9.80521299123423,3.57425782911967));
#20882=CARTESIAN_POINT('Ctrl Pts',(11.9668350211295,11.9287659082934,3.34323666910062));
#20883=CARTESIAN_POINT('Ctrl Pts',(13.8834175105647,14.052299961954,3.11226431322855));
#20884=CARTESIAN_POINT('Ctrl Pts',(15.8,16.1758528790132,2.8812431532095));
#20885=CARTESIAN_POINT('Ctrl Pts',(10.0502525316942,9.71169428155717,3.47602249721153));
#20886=CARTESIAN_POINT('Ctrl Pts',(11.9668350211295,11.8094568448422,3.23326515211327));
#20887=CARTESIAN_POINT('Ctrl Pts',(13.8834175105647,13.9072965714997,2.99011502771358));
#20888=CARTESIAN_POINT('Ctrl Pts',(15.8,16.0050591347847,2.74735768261532));
#20889=CARTESIAN_POINT('Ctrl Pts',(10.0502525316942,9.64719632995104,3.41409722674601));
#20890=CARTESIAN_POINT('Ctrl Pts',(11.9668350211295,11.7274687236956,3.16465335082919));
#20891=CARTESIAN_POINT('Ctrl Pts',(13.8834175105648,13.8077428217682,2.91499625447087));
#20892=CARTESIAN_POINT('Ctrl Pts',(15.8,15.8880152155128,2.66555237855405));
#20893=CARTESIAN_POINT('Ctrl Pts',(10.0502525316942,9.53672408685998,3.30251999207182));
#20894=CARTESIAN_POINT('Ctrl Pts',(11.9668350211294,11.58577497799,3.04246362184767));
#20895=CARTESIAN_POINT('Ctrl Pts',(13.8834175105647,13.6349367240444,2.78215337892879));
#20896=CARTESIAN_POINT('Ctrl Pts',(15.8,15.6839876151744,2.52209700870464));
#20897=CARTESIAN_POINT('Ctrl Pts',(10.0502525316942,9.36058107581317,3.09139659750778));
#20898=CARTESIAN_POINT('Ctrl Pts',(11.9668350211295,11.357410148179,2.80829724126977));
#20899=CARTESIAN_POINT('Ctrl Pts',(13.8834175105647,13.3541948572957,2.52507603204707));
#20900=CARTESIAN_POINT('Ctrl Pts',(15.8,15.3510239296616,2.24197667580906));
#20901=CARTESIAN_POINT('Ctrl Pts',(10.0502525316942,9.14733948977136,2.94903314862295));
#20902=CARTESIAN_POINT('Ctrl Pts',(11.9668350211294,11.0909774008914,2.65653626154119));
#20903=CARTESIAN_POINT('Ctrl Pts',(13.8834175105647,13.0346322911662,2.3639289644162));
#20904=CARTESIAN_POINT('Ctrl Pts',(15.8,14.9782702022862,2.07143207733445));
#20905=CARTESIAN_POINT('Ctrl Pts',(10.0502525316942,8.92650608260145,2.83936642791009));
#20906=CARTESIAN_POINT('Ctrl Pts',(11.9668350211294,10.8177624863471,2.54644119432445));
#20907=CARTESIAN_POINT('Ctrl Pts',(13.8834175105648,12.7090406610097,2.25343349088951));
#20908=CARTESIAN_POINT('Ctrl Pts',(15.8,14.6002970647553,1.96050825730386));
#20909=CARTESIAN_POINT('Ctrl Pts',(10.0502525316942,8.80866270544546,2.80374461319022));
#20910=CARTESIAN_POINT('Ctrl Pts',(11.9668350211294,10.6741860277864,2.51464388608039));
#20911=CARTESIAN_POINT('Ctrl Pts',(13.8834175105647,12.5396724561545,2.22549660720977));
#20912=CARTESIAN_POINT('Ctrl Pts',(15.8,14.4051957784954,1.93639588009994));
#20913=CARTESIAN_POINT('Ctrl Pts',(10.0502525316942,8.7276078365385,2.78743136471945));
#20914=CARTESIAN_POINT('Ctrl Pts',(11.9668350211294,10.5761285330411,2.50261311086535));
#20915=CARTESIAN_POINT('Ctrl Pts',(13.8834175105647,12.4246492295437,2.21779485701125));
#20916=CARTESIAN_POINT('Ctrl Pts',(15.8,14.2731699260464,1.93297660315714));
#20917=CARTESIAN_POINT('Ctrl Pts',(15.8,14.3165490635069,1.93458023611785));
#20918=CARTESIAN_POINT('Ctrl Pts',(15.8,14.3078898665466,1.93416388872989));
#20919=CARTESIAN_POINT('Ctrl Pts',(15.8,14.2992223526576,1.93379536300002));
#20920=CARTESIAN_POINT('Ctrl Pts',(15.8,14.2905465237881,1.93347464492456));
#20921=CARTESIAN_POINT('Ctrl Pts',(15.8,14.2818623815451,1.93320172507161));
#20922=CARTESIAN_POINT('Ctrl Pts',(15.8,14.2731699260464,1.93297660315714));
#20923=CARTESIAN_POINT('Origin',(15.8,14.6809722990553,3.35534058166953));
#20924=CARTESIAN_POINT('Ctrl Pts',(10.0502525316942,10.6909231138624,1.22531840158854));
#20925=CARTESIAN_POINT('Ctrl Pts',(11.9668350211294,12.7560692212929,0.476385041699011));
#20926=CARTESIAN_POINT('Ctrl Pts',(13.8834175105647,14.8212153287235,-0.272548318190523));
#20927=CARTESIAN_POINT('Ctrl Pts',(15.8,16.886361436154,-1.02148167808006));
#20928=CARTESIAN_POINT('Ctrl Pts',(10.0502525316942,10.6687583477967,0.951811288039439));
#20929=CARTESIAN_POINT('Ctrl Pts',(11.9668350211294,12.7082628707158,0.160771418505769));
#20930=CARTESIAN_POINT('Ctrl Pts',(13.8834175105647,14.7477045483503,-0.630916858166452));
#20931=CARTESIAN_POINT('Ctrl Pts',(15.8,16.7872090712694,-1.42195672770012));
#20932=CARTESIAN_POINT('Ctrl Pts',(10.0502525316942,10.5909841198542,0.538737970192933));
#20933=CARTESIAN_POINT('Ctrl Pts',(11.9668350211295,12.5832583421986,-0.315735593698355));
#20934=CARTESIAN_POINT('Ctrl Pts',(13.8834175105647,14.5756107736058,-1.16942659814004));
#20935=CARTESIAN_POINT('Ctrl Pts',(15.8,16.5678849959503,-2.02390016203133));
#20936=CARTESIAN_POINT('Ctrl Pts',(10.0502525316942,10.4118557126012,0.350797420983487));
#20937=CARTESIAN_POINT('Ctrl Pts',(11.9668350211295,12.3552036734465,-0.527317792292714));
#20938=CARTESIAN_POINT('Ctrl Pts',(13.8834175105647,14.2985259967778,-1.40583184426593));
#20939=CARTESIAN_POINT('Ctrl Pts',(15.8,16.2418739576232,-2.28394705754213));
#20940=CARTESIAN_POINT('Ctrl Pts',(10.0502525316942,10.2498870013208,0.276502431596345));
#20941=CARTESIAN_POINT('Ctrl Pts',(11.9668350211295,12.1559807242605,-0.603405794214879));
#20942=CARTESIAN_POINT('Ctrl Pts',(13.8834175105647,14.0620012424206,-1.48361038150706));
#20943=CARTESIAN_POINT('Ctrl Pts',(15.8,15.9680949653604,-2.36351860731828));
#20944=CARTESIAN_POINT('Ctrl Pts',(10.0502525316942,10.0905890686414,0.193479460458704));
#20945=CARTESIAN_POINT('Ctrl Pts',(11.9668350211294,11.9589846875421,-0.687106219194374));
#20946=CARTESIAN_POINT('Ctrl Pts',(13.8834175105647,13.8273908205778,-1.56802487912709));
#20947=CARTESIAN_POINT('Ctrl Pts',(15.8,15.6957864394785,-2.44861055878017));
#20948=CARTESIAN_POINT('Ctrl Pts',(10.0502525316942,9.85767148446325,0.0477779613143544));
#20949=CARTESIAN_POINT('Ctrl Pts',(11.9668350211294,11.6692901486065,-0.83847512310783));
#20950=CARTESIAN_POINT('Ctrl Pts',(13.8834175105647,13.4808398643785,-1.72481200902093));
#20951=CARTESIAN_POINT('Ctrl Pts',(15.8,15.2924585285217,-2.61106509344312));
#20952=CARTESIAN_POINT('Ctrl Pts',(10.0502525316942,9.61095465953459,-0.0220599042734161));
#20953=CARTESIAN_POINT('Ctrl Pts',(11.9668350211294,11.3690757684926,-0.900879773662285));
#20954=CARTESIAN_POINT('Ctrl Pts',(13.8834175105647,13.1271782591657,-1.77979551853006));
#20955=CARTESIAN_POINT('Ctrl Pts',(15.8,14.8852993681237,-2.65861538791893));
#20956=CARTESIAN_POINT('Ctrl Pts',(10.0502525316942,9.36700900338232,-0.0579833517275561));
#20957=CARTESIAN_POINT('Ctrl Pts',(11.9668350211294,11.07518337287,-0.920984711114089));
#20958=CARTESIAN_POINT('Ctrl Pts',(13.8834175105647,12.7833535968728,-1.78409102238058));
#20959=CARTESIAN_POINT('Ctrl Pts',(15.8,14.4915279663605,-2.64709238176711));
#20960=CARTESIAN_POINT('Ctrl Pts',(10.0502525316942,9.243940799223,-0.0555068892974567));
#20961=CARTESIAN_POINT('Ctrl Pts',(11.9668350211294,10.9288207869826,-0.906948929192822));
#20962=CARTESIAN_POINT('Ctrl Pts',(13.8834175105647,12.6136545606744,-1.75838634306183));
#20963=CARTESIAN_POINT('Ctrl Pts',(15.8,14.298534548434,-2.6098283829572));
#20964=CARTESIAN_POINT('Ctrl Pts',(10.0502525316942,9.16181196696065,-0.0459743785884358));
#20965=CARTESIAN_POINT('Ctrl Pts',(11.9668350211294,10.8318459401268,-0.888076944549314));
#20966=CARTESIAN_POINT('Ctrl Pts',(13.8834175105647,12.501879913293,-1.73017951051019));
#20967=CARTESIAN_POINT('Ctrl Pts',(15.8,14.1719138864591,-2.57228207647107));
#20968=CARTESIAN_POINT('Ctrl Pts',(15.8,14.2136654476498,-2.58416182157067));
#20969=CARTESIAN_POINT('Ctrl Pts',(15.8,14.2053014035364,-2.58188195244865));
#20970=CARTESIAN_POINT('Ctrl Pts',(15.8,14.1969442272588,-2.57955403215479));
#20971=CARTESIAN_POINT('Ctrl Pts',(15.8,14.1885939163425,-2.57717807460939));
#20972=CARTESIAN_POINT('Ctrl Pts',(15.8,14.1802504694012,-2.57475408927931));
#20973=CARTESIAN_POINT('Ctrl Pts',(15.8,14.1719138864591,-2.57228207647107));
#20974=CARTESIAN_POINT('Origin',(15.8,14.999291632217,-1.34555140976955));
#20975=CARTESIAN_POINT('Origin',(21.,10.,0.));
#20976=CARTESIAN_POINT('',(0.,0.,0.));
#20977=CARTESIAN_POINT('Origin',(21.,-6.,-7.));
#20978=CARTESIAN_POINT('',(21.,-5.5,-2.39791576165636));
#20979=CARTESIAN_POINT('',(21.,-6.,-7.34788079488412E-16));
#20980=CARTESIAN_POINT('Origin',(21.,0.,0.));
#20981=CARTESIAN_POINT('',(21.,-5.5,2.39791576165636));
#20982=CARTESIAN_POINT('',(21.,-5.5,7.));
#20983=CARTESIAN_POINT('Origin',(21.,0.,0.));
#20984=CARTESIAN_POINT('Origin',(28.,-6.,7.));
#20985=CARTESIAN_POINT('',(28.,-5.5,2.39791576165636));
#20986=CARTESIAN_POINT('',(28.,-6.,-7.34788079488412E-16));
#20987=CARTESIAN_POINT('Origin',(28.,0.,0.));
#20988=CARTESIAN_POINT('',(28.,-5.5,-2.39791576165636));
#20989=CARTESIAN_POINT('',(28.,-5.5,-7.));
#20990=CARTESIAN_POINT('Origin',(28.,0.,0.));
#20991=CARTESIAN_POINT('Origin',(24.5,-5.5,0.));
#20992=CARTESIAN_POINT('',(47.5,-5.5,-2.39791576165636));
#20993=CARTESIAN_POINT('',(47.5,-5.5,2.39791576165636));
#20994=CARTESIAN_POINT('Origin',(21.,7.,6.));
#20995=CARTESIAN_POINT('',(21.,-2.39791576165636,5.5));
#20996=CARTESIAN_POINT('',(21.,2.39791576165636,5.5));
#20997=CARTESIAN_POINT('Origin',(21.,0.,0.));
#20998=CARTESIAN_POINT('',(21.,7.,5.5));
#20999=CARTESIAN_POINT('Origin',(24.5,0.,5.5));
#21000=CARTESIAN_POINT('',(28.,-2.39791576165636,5.5));
#21001=CARTESIAN_POINT('',(47.5,-2.39791576165636,5.5));
#21002=CARTESIAN_POINT('',(28.,2.39791576165636,5.5));
#21003=CARTESIAN_POINT('',(28.,-7.,5.5));
#21004=CARTESIAN_POINT('',(47.5,2.39791576165636,5.5));
#21005=CARTESIAN_POINT('Origin',(28.,-7.,6.));
#21006=CARTESIAN_POINT('Origin',(28.,0.,0.));
#21007=CARTESIAN_POINT('Origin',(84.139375,0.,0.));
#21008=CARTESIAN_POINT('',(83.77875,0.,0.));
#21009=CARTESIAN_POINT('',(84.5,-1.25,-1.53080849893419E-16));
#21010=CARTESIAN_POINT('',(84.139375,-0.625,-7.65404249467096E-17));
#21011=CARTESIAN_POINT('Origin',(84.5,0.,0.));
#21012=CARTESIAN_POINT('Origin',(84.75,0.,0.));
#21013=CARTESIAN_POINT('',(85.,-1.25,-1.53080849893419E-16));
#21014=CARTESIAN_POINT('',(84.75,-1.25,-1.53080849893419E-16));
#21015=CARTESIAN_POINT('Origin',(85.,0.,0.));
#21016=CARTESIAN_POINT('Origin',(10.25,0.,0.));
#21017=CARTESIAN_POINT('',(10.,-1.25,-1.53080849893419E-16));
#21018=CARTESIAN_POINT('Origin',(10.,0.,0.));
#21019=CARTESIAN_POINT('',(10.5,-1.25,-1.53080849893419E-16));
#21020=CARTESIAN_POINT('',(10.25,-1.25,-1.53080849893419E-16));
#21021=CARTESIAN_POINT('Origin',(10.5,0.,0.));
#21022=CARTESIAN_POINT('Origin',(10.5,0.,0.));
#21023=CARTESIAN_POINT('',(11.22125,0.,0.));
#21024=CARTESIAN_POINT('',(10.5,-1.25,-1.53080849893419E-16));
#21025=CARTESIAN_POINT('Origin',(10.,5.2,0.));
#21026=CARTESIAN_POINT('',(10.,-5.2,-6.36816335556624E-16));
#21027=CARTESIAN_POINT('Origin',(10.,0.,0.));
#21028=CARTESIAN_POINT('Origin',(10.4,0.,0.));
#21029=CARTESIAN_POINT('',(10.8,-6.,-7.34788079488412E-16));
#21030=CARTESIAN_POINT('Origin',(10.8,0.,0.));
#21031=CARTESIAN_POINT('',(10.4,-5.6,-6.85802207522518E-16));
#21032=CARTESIAN_POINT('Origin',(47.5,0.,0.));
#21033=CARTESIAN_POINT('',(84.2,-6.,-7.34788079488412E-16));
#21034=CARTESIAN_POINT('Origin',(84.2,0.,0.));
#21035=CARTESIAN_POINT('',(47.5,-6.,-7.34788079488412E-16));
#21036=CARTESIAN_POINT('',(47.5,-6.,-7.34788079488412E-16));
#21037=CARTESIAN_POINT('Origin',(84.6,0.,0.));
#21038=CARTESIAN_POINT('',(85.,-5.2,-6.36816335556624E-16));
#21039=CARTESIAN_POINT('Origin',(85.,0.,0.));
#21040=CARTESIAN_POINT('',(84.6,-5.6,-6.85802207522518E-16));
#21041=CARTESIAN_POINT('Origin',(85.,0.,0.));
#21042=CARTESIAN_POINT('',(0.,0.,0.));
#21043=CARTESIAN_POINT('Origin',(21.,-6.,-7.));
#21044=CARTESIAN_POINT('',(21.,-5.5,-2.39791576165636));
#21045=CARTESIAN_POINT('',(21.,-6.,-7.34788079488412E-16));
#21046=CARTESIAN_POINT('Origin',(21.,0.,0.));
#21047=CARTESIAN_POINT('',(21.,-5.5,2.39791576165636));
#21048=CARTESIAN_POINT('',(21.,-5.5,7.));
#21049=CARTESIAN_POINT('Origin',(21.,0.,0.));
#21050=CARTESIAN_POINT('Origin',(28.,-6.,7.));
#21051=CARTESIAN_POINT('',(28.,-5.5,2.39791576165636));
#21052=CARTESIAN_POINT('',(28.,-6.,-7.34788079488412E-16));
#21053=CARTESIAN_POINT('Origin',(28.,0.,0.));
#21054=CARTESIAN_POINT('',(28.,-5.5,-2.39791576165636));
#21055=CARTESIAN_POINT('',(28.,-5.5,-7.));
#21056=CARTESIAN_POINT('Origin',(28.,0.,0.));
#21057=CARTESIAN_POINT('Origin',(24.5,-5.5,0.));
#21058=CARTESIAN_POINT('',(0.,-5.5,-2.39791576165636));
#21059=CARTESIAN_POINT('',(0.,-5.5,2.39791576165636));
#21060=CARTESIAN_POINT('Origin',(21.,7.,6.));
#21061=CARTESIAN_POINT('',(21.,-2.39791576165636,5.5));
#21062=CARTESIAN_POINT('',(21.,2.39791576165636,5.5));
#21063=CARTESIAN_POINT('Origin',(21.,0.,0.));
#21064=CARTESIAN_POINT('',(21.,7.,5.5));
#21065=CARTESIAN_POINT('Origin',(24.5,0.,5.5));
#21066=CARTESIAN_POINT('',(28.,-2.39791576165636,5.5));
#21067=CARTESIAN_POINT('',(0.,-2.39791576165636,5.5));
#21068=CARTESIAN_POINT('',(28.,2.39791576165636,5.5));
#21069=CARTESIAN_POINT('',(28.,-7.,5.5));
#21070=CARTESIAN_POINT('',(0.,2.39791576165636,5.5));
#21071=CARTESIAN_POINT('Origin',(28.,-7.,6.));
#21072=CARTESIAN_POINT('Origin',(28.,0.,0.));
#21073=CARTESIAN_POINT('Origin',(89.139375,0.,0.));
#21074=CARTESIAN_POINT('',(88.77875,0.,0.));
#21075=CARTESIAN_POINT('',(89.5,-1.25,-1.53080849893419E-16));
#21076=CARTESIAN_POINT('',(89.139375,-0.625,-7.65404249467096E-17));
#21077=CARTESIAN_POINT('Origin',(89.5,0.,0.));
#21078=CARTESIAN_POINT('Origin',(89.75,0.,0.));
#21079=CARTESIAN_POINT('',(90.,-1.25,-1.53080849893419E-16));
#21080=CARTESIAN_POINT('',(89.75,-1.25,-1.53080849893419E-16));
#21081=CARTESIAN_POINT('Origin',(90.,0.,0.));
#21082=CARTESIAN_POINT('Origin',(-89.75,0.,0.));
#21083=CARTESIAN_POINT('',(-90.,-1.25,-1.53080849893419E-16));
#21084=CARTESIAN_POINT('Origin',(-90.,0.,0.));
#21085=CARTESIAN_POINT('',(-89.5,-1.25,-1.53080849893419E-16));
#21086=CARTESIAN_POINT('',(-89.75,-1.25,-1.53080849893419E-16));
#21087=CARTESIAN_POINT('Origin',(-89.5,0.,0.));
#21088=CARTESIAN_POINT('Origin',(-89.5,0.,0.));
#21089=CARTESIAN_POINT('',(-88.77875,0.,0.));
#21090=CARTESIAN_POINT('',(-89.5,-1.25,-1.53080849893419E-16));
#21091=CARTESIAN_POINT('Origin',(-90.,5.2,0.));
#21092=CARTESIAN_POINT('',(-90.,-5.2,-6.36816335556624E-16));
#21093=CARTESIAN_POINT('Origin',(-90.,0.,0.));
#21094=CARTESIAN_POINT('Origin',(-89.6,0.,0.));
#21095=CARTESIAN_POINT('',(-89.2,-6.,-7.34788079488411E-16));
#21096=CARTESIAN_POINT('Origin',(-89.2,0.,0.));
#21097=CARTESIAN_POINT('',(-89.6,-5.6,-6.85802207522518E-16));
#21098=CARTESIAN_POINT('Origin',(0.,0.,0.));
#21099=CARTESIAN_POINT('',(89.2,-6.,-7.34788079488412E-16));
#21100=CARTESIAN_POINT('Origin',(89.2,0.,0.));
#21101=CARTESIAN_POINT('',(0.,-6.,-7.34788079488412E-16));
#21102=CARTESIAN_POINT('',(0.,-6.,-7.34788079488412E-16));
#21103=CARTESIAN_POINT('Origin',(89.6,0.,0.));
#21104=CARTESIAN_POINT('',(90.,-5.2,-6.36816335556624E-16));
#21105=CARTESIAN_POINT('Origin',(90.,0.,0.));
#21106=CARTESIAN_POINT('',(89.6,-5.6,-6.85802207522518E-16));
#21107=CARTESIAN_POINT('Origin',(90.,0.,0.));
#21108=CARTESIAN_POINT('',(0.,0.,0.));
#21109=CARTESIAN_POINT('Origin',(4.,8.09016994374947,-5.87785252292473));
#21110=CARTESIAN_POINT('',(4.,9.48983357577093,-3.95138080506939));
#21111=CARTESIAN_POINT('',(4.,6.69050631172802,-7.80432424078008));
#21112=CARTESIAN_POINT('Origin',(4.,8.09016994374947,-5.87785252292473));
#21113=CARTESIAN_POINT('',(2.36305161962877,9.25963747468151,-7.15186086536042));
#21114=CARTESIAN_POINT('',(2.36305161962877,9.66320922106503,-6.59639201002517));
#21115=CARTESIAN_POINT('Ctrl Pts',(2.36305161962876,9.25963747468151,-7.15186086536042));
#21116=CARTESIAN_POINT('Ctrl Pts',(2.34215062955512,9.33091437868292,-7.05957742979088));
#21117=CARTESIAN_POINT('Ctrl Pts',(2.33256137669178,9.40089182481285,-6.96601137146006));
#21118=CARTESIAN_POINT('Ctrl Pts',(2.33256137669178,9.53010584356091,-6.78816353218381));
#21119=CARTESIAN_POINT('Ctrl Pts',(2.34215062955512,9.59746823296338,-6.69269752392735));
#21120=CARTESIAN_POINT('Ctrl Pts',(2.36305161962876,9.66320922106503,-6.59639201002516));
#21121=CARTESIAN_POINT('',(5.63694838037123,9.25963747468151,-7.15186086536042));
#21122=CARTESIAN_POINT('Ctrl Pts',(5.63694838037123,9.25963747468149,-7.15186086536043));
#21123=CARTESIAN_POINT('Ctrl Pts',(5.43435664662035,9.41577612470672,-7.26884057730417));
#21124=CARTESIAN_POINT('Ctrl Pts',(5.15858882449494,9.55944543027121,-7.37642824958397));
#21125=CARTESIAN_POINT('Ctrl Pts',(4.63402456511048,9.73338541206091,-7.5066654368745));
#21126=CARTESIAN_POINT('Ctrl Pts',(4.2912458937239,9.7879741784414,-7.54752684540867));
#21127=CARTESIAN_POINT('Ctrl Pts',(4.,9.7879741784414,-7.54752684540867));
#21128=CARTESIAN_POINT('Ctrl Pts',(3.7087541062761,9.7879741784414,-7.54752684540867));
#21129=CARTESIAN_POINT('Ctrl Pts',(3.36597543488952,9.73338541206091,-7.5066654368745));
#21130=CARTESIAN_POINT('Ctrl Pts',(2.84141117550506,9.55944543027121,-7.37642824958397));
#21131=CARTESIAN_POINT('Ctrl Pts',(2.56564335337965,9.41577612470672,-7.26884057730417));
#21132=CARTESIAN_POINT('Ctrl Pts',(2.36305161962877,9.25963747468149,-7.15186086536043));
#21133=CARTESIAN_POINT('',(5.63694838037123,9.66320922106503,-6.59639201002517));
#21134=CARTESIAN_POINT('Ctrl Pts',(5.63694838037123,9.66320922106503,-6.59639201002517));
#21135=CARTESIAN_POINT('Ctrl Pts',(5.64480038182766,9.6077764900278,-6.69985819864571));
#21136=CARTESIAN_POINT('Ctrl Pts',(5.64846349832042,9.5458342503805,-6.79782963077036));
#21137=CARTESIAN_POINT('Ctrl Pts',(5.64846349832042,9.41494517586244,-6.97798298652422));
#21138=CARTESIAN_POINT('Ctrl Pts',(5.64480038182766,9.34091001165019,-7.06716839466448));
#21139=CARTESIAN_POINT('Ctrl Pts',(5.63694838037123,9.25963747468151,-7.15186086536042));
#21140=CARTESIAN_POINT('Ctrl Pts',(2.36305161962877,9.66320922106504,-6.59639201002515));
#21141=CARTESIAN_POINT('Ctrl Pts',(2.56564335337965,9.82271303472001,-6.70873997158947));
#21142=CARTESIAN_POINT('Ctrl Pts',(2.84141117550506,9.96943124850423,-6.81213118171848));
#21143=CARTESIAN_POINT('Ctrl Pts',(3.36597543488952,10.1470445845151,-6.93731243067146));
#21144=CARTESIAN_POINT('Ctrl Pts',(3.7087541062761,10.2027749498801,-6.97660256300298));
#21145=CARTESIAN_POINT('Ctrl Pts',(4.,10.2027749498801,-6.97660256300298));
#21146=CARTESIAN_POINT('Ctrl Pts',(4.2912458937239,10.2027749498801,-6.97660256300298));
#21147=CARTESIAN_POINT('Ctrl Pts',(4.63402456511048,10.1470445845151,-6.93731243067146));
#21148=CARTESIAN_POINT('Ctrl Pts',(5.15858882449494,9.96943124850423,-6.81213118171848));
#21149=CARTESIAN_POINT('Ctrl Pts',(5.43435664662035,9.82271303472001,-6.70873997158947));
#21150=CARTESIAN_POINT('Ctrl Pts',(5.63694838037123,9.66320922106504,-6.59639201002515));
#21151=CARTESIAN_POINT('',(5.63694838037123,6.54081691696393,-5.10957082921438));
#21152=CARTESIAN_POINT('',(5.63694838037123,6.88071421703296,-4.64174233058239));
#21153=CARTESIAN_POINT('Ctrl Pts',(5.63694838037124,6.54081691696393,-5.10957082921438));
#21154=CARTESIAN_POINT('Ctrl Pts',(5.6577376463315,6.60095637772735,-5.03258565462996));
#21155=CARTESIAN_POINT('Ctrl Pts',(5.66743862330822,6.66027285287123,-4.95372427854694));
#21156=CARTESIAN_POINT('Ctrl Pts',(5.66743862330822,6.7694092537529,-4.80351090950812));
#21157=CARTESIAN_POINT('Ctrl Pts',(5.6577376463315,6.82608108049478,-4.72272808388943));
#21158=CARTESIAN_POINT('Ctrl Pts',(5.63694838037124,6.88071421703297,-4.64174233058239));
#21159=CARTESIAN_POINT('',(2.36305161962877,6.54081691696392,-5.10957082921439));
#21160=CARTESIAN_POINT('Ctrl Pts',(2.36305161962877,6.54081691696392,-5.10957082921439));
#21161=CARTESIAN_POINT('Ctrl Pts',(2.56564497161068,6.38499222767917,-4.99215633639486));
#21162=CARTESIAN_POINT('Ctrl Pts',(2.8414185613243,6.24167414543094,-4.88407927525699));
#21163=CARTESIAN_POINT('Ctrl Pts',(3.36598484931781,6.06819253427498,-4.75321678286295));
#21164=CARTESIAN_POINT('Ctrl Pts',(3.70875810561651,6.0137647807275,-4.71213679365121));
#21165=CARTESIAN_POINT('Ctrl Pts',(4.29124189438349,6.0137647807275,-4.71213679365121));
#21166=CARTESIAN_POINT('Ctrl Pts',(4.6340151506822,6.06819253427498,-4.75321678286295));
#21167=CARTESIAN_POINT('Ctrl Pts',(5.1585814386757,6.24167414543094,-4.88407927525699));
#21168=CARTESIAN_POINT('Ctrl Pts',(5.43435502838932,6.38499222767917,-4.99215633639486));
#21169=CARTESIAN_POINT('Ctrl Pts',(5.63694838037123,6.54081691696391,-5.10957082921439));
#21170=CARTESIAN_POINT('',(2.36305161962877,6.88071421703297,-4.64174233058238));
#21171=CARTESIAN_POINT('Ctrl Pts',(2.36305161962877,6.88071421703297,-4.64174233058238));
#21172=CARTESIAN_POINT('Ctrl Pts',(2.3422623536685,6.82608108049479,-4.72272808388942));
#21173=CARTESIAN_POINT('Ctrl Pts',(2.33256137669178,6.7694092537529,-4.80351090950811));
#21174=CARTESIAN_POINT('Ctrl Pts',(2.33256137669178,6.66027285287122,-4.95372427854695));
#21175=CARTESIAN_POINT('Ctrl Pts',(2.3422623536685,6.60095637772735,-5.03258565462997));
#21176=CARTESIAN_POINT('Ctrl Pts',(2.36305161962877,6.54081691696392,-5.10957082921439));
#21177=CARTESIAN_POINT('Ctrl Pts',(5.63694838037123,6.88071421703298,-4.64174233058237));
#21178=CARTESIAN_POINT('Ctrl Pts',(5.43435502838932,6.72089392139729,-4.5298273181056));
#21179=CARTESIAN_POINT('Ctrl Pts',(5.1585814386757,6.57381880512416,-4.4269213706742));
#21180=CARTESIAN_POINT('Ctrl Pts',(4.6340151506822,6.39575241293544,-4.30236928800296));
#21181=CARTESIAN_POINT('Ctrl Pts',(4.29124189438349,6.33986392069446,-4.2632998331195));
#21182=CARTESIAN_POINT('Ctrl Pts',(3.70875810561651,6.33986392069446,-4.2632998331195));
#21183=CARTESIAN_POINT('Ctrl Pts',(3.36598484931781,6.39575241293544,-4.30236928800296));
#21184=CARTESIAN_POINT('Ctrl Pts',(2.8414185613243,6.57381880512416,-4.4269213706742));
#21185=CARTESIAN_POINT('Ctrl Pts',(2.56564497161068,6.72089392139729,-4.5298273181056));
#21186=CARTESIAN_POINT('Ctrl Pts',(2.36305161962877,6.88071421703298,-4.64174233058237));
#21187=CARTESIAN_POINT('Origin',(5.91847419018562,0.,0.));
#21188=CARTESIAN_POINT('',(6.2,-12.6,-1.54305496692567E-15));
#21189=CARTESIAN_POINT('Origin',(6.2,0.,0.));
#21190=CARTESIAN_POINT('',(5.64846349832042,-11.7184061386079,-5.83505075665543E-17));
#21191=CARTESIAN_POINT('',(5.91847419018562,-12.15,-1.48794586096403E-15));
#21192=CARTESIAN_POINT('',(5.63694838037123,-11.694962421875,0.343298632289184));
#21193=CARTESIAN_POINT('Ctrl Pts',(5.64846349832042,-11.7184061386079,1.31838984174237E-15));
#21194=CARTESIAN_POINT('Ctrl Pts',(5.64846349832042,-11.7184061386079,0.11134089704324));
#21195=CARTESIAN_POINT('Ctrl Pts',(5.64480038182766,-11.7109323002033,0.227010185553986));
#21196=CARTESIAN_POINT('Ctrl Pts',(5.63694838037123,-11.694962421875,0.343298632289185));
#21197=CARTESIAN_POINT('',(5.63694838037123,-9.66320922106502,6.59639201002516));
#21198=CARTESIAN_POINT('Origin',(5.63694838037123,0.,0.));
#21199=CARTESIAN_POINT('',(5.63694838037123,-9.25963747468151,7.15186086536042));
#21200=CARTESIAN_POINT('Ctrl Pts',(5.63694838037123,-9.66320922106503,6.59639201002517));
#21201=CARTESIAN_POINT('Ctrl Pts',(5.64480038182766,-9.6077764900278,6.69985819864571));
#21202=CARTESIAN_POINT('Ctrl Pts',(5.64846349832042,-9.5458342503805,6.79782963077036));
#21203=CARTESIAN_POINT('Ctrl Pts',(5.64846349832042,-9.41494517586244,6.97798298652422));
#21204=CARTESIAN_POINT('Ctrl Pts',(5.64480038182766,-9.34091001165019,7.06716839466448));
#21205=CARTESIAN_POINT('Ctrl Pts',(5.63694838037123,-9.25963747468151,7.15186086536042));
#21206=CARTESIAN_POINT('',(5.63694838037123,-3.94043853820961,11.0164851076281));
#21207=CARTESIAN_POINT('Origin',(5.63694838037123,0.,0.));
#21208=CARTESIAN_POINT('',(5.63694838037123,-3.28744573566193,11.2286553306742));
#21209=CARTESIAN_POINT('Ctrl Pts',(5.63694838037123,-3.94043853820961,11.0164851076281));
#21210=CARTESIAN_POINT('Ctrl Pts',(5.64480038182766,-3.83477661697381,11.0676084707674));
#21211=CARTESIAN_POINT('Ctrl Pts',(5.64846349832042,-3.72707812948065,11.1104602893608));
#21212=CARTESIAN_POINT('Ctrl Pts',(5.64846349832042,-3.51529515815442,11.1792727480714));
#21213=CARTESIAN_POINT('Ctrl Pts',(5.64480038182766,-3.40297758450084,11.2079084812322));
#21214=CARTESIAN_POINT('Ctrl Pts',(5.63694838037123,-3.28744573566193,11.2286553306742));
#21215=CARTESIAN_POINT('',(5.63694838037123,3.28744573566193,11.2286553306742));
#21216=CARTESIAN_POINT('Origin',(5.63694838037123,0.,0.));
#21217=CARTESIAN_POINT('',(5.63694838037123,3.94043853820961,11.0164851076281));
#21218=CARTESIAN_POINT('Ctrl Pts',(5.63694838037123,3.28744573566193,11.2286553306742));
#21219=CARTESIAN_POINT('Ctrl Pts',(5.64480038182766,3.40297758450084,11.2079084812322));
#21220=CARTESIAN_POINT('Ctrl Pts',(5.64846349832042,3.51529515815442,11.1792727480715));
#21221=CARTESIAN_POINT('Ctrl Pts',(5.64846349832042,3.72707812948066,11.1104602893608));
#21222=CARTESIAN_POINT('Ctrl Pts',(5.64480038182766,3.83477661697381,11.0676084707674));
#21223=CARTESIAN_POINT('Ctrl Pts',(5.63694838037123,3.94043853820961,11.0164851076281));
#21224=CARTESIAN_POINT('',(5.63694838037123,9.25963747468151,7.15186086536041));
#21225=CARTESIAN_POINT('Origin',(5.63694838037123,0.,0.));
#21226=CARTESIAN_POINT('',(5.63694838037123,9.66320922106503,6.59639201002516));
#21227=CARTESIAN_POINT('Ctrl Pts',(5.63694838037123,9.25963747468151,7.15186086536041));
#21228=CARTESIAN_POINT('Ctrl Pts',(5.64480038182766,9.34091001165019,7.06716839466447));
#21229=CARTESIAN_POINT('Ctrl Pts',(5.64846349832042,9.41494517586244,6.97798298652422));
#21230=CARTESIAN_POINT('Ctrl Pts',(5.64846349832042,9.5458342503805,6.79782963077036));
#21231=CARTESIAN_POINT('Ctrl Pts',(5.64480038182766,9.6077764900278,6.69985819864571));
#21232=CARTESIAN_POINT('Ctrl Pts',(5.63694838037123,9.66320922106503,6.59639201002516));
#21233=CARTESIAN_POINT('',(5.63694838037123,11.694962421875,0.343298632289183));
#21234=CARTESIAN_POINT('Origin',(5.63694838037123,0.,0.));
#21235=CARTESIAN_POINT('',(5.63694838037123,11.694962421875,-0.343298632289183));
#21236=CARTESIAN_POINT('Ctrl Pts',(5.63694838037123,11.694962421875,0.343298632289183));
#21237=CARTESIAN_POINT('Ctrl Pts',(5.64480038182766,11.7109323002033,0.227010185553984));
#21238=CARTESIAN_POINT('Ctrl Pts',(5.64846349832042,11.7184061386079,0.111340897043238));
#21239=CARTESIAN_POINT('Ctrl Pts',(5.64846349832042,11.7184061386079,-0.111340897043237));
#21240=CARTESIAN_POINT('Ctrl Pts',(5.64480038182766,11.7109323002033,-0.227010185553985));
#21241=CARTESIAN_POINT('Ctrl Pts',(5.63694838037123,11.694962421875,-0.343298632289183));
#21242=CARTESIAN_POINT('Origin',(5.63694838037123,0.,0.));
#21243=CARTESIAN_POINT('',(5.63694838037123,3.94043853820961,-11.0164851076281));
#21244=CARTESIAN_POINT('Origin',(5.63694838037123,0.,0.));
#21245=CARTESIAN_POINT('',(5.63694838037123,3.28744573566193,-11.2286553306742));
#21246=CARTESIAN_POINT('Ctrl Pts',(5.63694838037123,3.94043853820961,-11.0164851076281));
#21247=CARTESIAN_POINT('Ctrl Pts',(5.64480038182766,3.83477661697381,-11.0676084707674));
#21248=CARTESIAN_POINT('Ctrl Pts',(5.64846349832042,3.72707812948065,-11.1104602893608));
#21249=CARTESIAN_POINT('Ctrl Pts',(5.64846349832042,3.51529515815441,-11.1792727480715));
#21250=CARTESIAN_POINT('Ctrl Pts',(5.64480038182766,3.40297758450083,-11.2079084812322));
#21251=CARTESIAN_POINT('Ctrl Pts',(5.63694838037123,3.28744573566193,-11.2286553306742));
#21252=CARTESIAN_POINT('',(5.63694838037123,-3.28744573566193,-11.2286553306742));
#21253=CARTESIAN_POINT('Origin',(5.63694838037123,0.,0.));
#21254=CARTESIAN_POINT('',(5.63694838037123,-3.94043853820961,-11.0164851076281));
#21255=CARTESIAN_POINT('Ctrl Pts',(5.63694838037123,-3.28744573566193,-11.2286553306742));
#21256=CARTESIAN_POINT('Ctrl Pts',(5.64480038182766,-3.40297758450084,-11.2079084812322));
#21257=CARTESIAN_POINT('Ctrl Pts',(5.64846349832042,-3.51529515815442,-11.1792727480715));
#21258=CARTESIAN_POINT('Ctrl Pts',(5.64846349832042,-3.72707812948065,-11.1104602893608));
#21259=CARTESIAN_POINT('Ctrl Pts',(5.64480038182766,-3.83477661697381,-11.0676084707674));
#21260=CARTESIAN_POINT('Ctrl Pts',(5.63694838037123,-3.94043853820961,-11.0164851076281));
#21261=CARTESIAN_POINT('',(5.63694838037123,-9.25963747468151,-7.15186086536041));
#21262=CARTESIAN_POINT('Origin',(5.63694838037123,0.,0.));
#21263=CARTESIAN_POINT('',(5.63694838037123,-9.66320922106503,-6.59639201002516));
#21264=CARTESIAN_POINT('Ctrl Pts',(5.63694838037123,-9.25963747468151,-7.15186086536042));
#21265=CARTESIAN_POINT('Ctrl Pts',(5.64480038182766,-9.34091001165019,-7.06716839466447));
#21266=CARTESIAN_POINT('Ctrl Pts',(5.64846349832042,-9.41494517586245,-6.97798298652421));
#21267=CARTESIAN_POINT('Ctrl Pts',(5.64846349832042,-9.54583425038051,-6.79782963077034));
#21268=CARTESIAN_POINT('Ctrl Pts',(5.64480038182766,-9.60777649002781,-6.6998581986457));
#21269=CARTESIAN_POINT('Ctrl Pts',(5.63694838037123,-9.66320922106503,-6.59639201002516));
#21270=CARTESIAN_POINT('',(5.63694838037123,-11.694962421875,-0.343298632289181));
#21271=CARTESIAN_POINT('Origin',(5.63694838037123,0.,0.));
#21272=CARTESIAN_POINT('Ctrl Pts',(5.63694838037123,-11.694962421875,-0.343298632289181));
#21273=CARTESIAN_POINT('Ctrl Pts',(5.64480038182766,-11.7109323002033,-0.227010185553983));
#21274=CARTESIAN_POINT('Ctrl Pts',(5.64846349832042,-11.7184061386079,-0.111340897043236));
#21275=CARTESIAN_POINT('Ctrl Pts',(5.64846349832042,-11.7184061386079,1.52655665885959E-15));
#21276=CARTESIAN_POINT('Origin',(4.,0.,0.));
#21277=CARTESIAN_POINT('',(2.36305161962877,3.94043853820961,-11.0164851076281));
#21278=CARTESIAN_POINT('Origin',(2.36305161962877,0.,0.));
#21279=CARTESIAN_POINT('Ctrl Pts',(2.36305161962877,3.94043853820962,-11.0164851076281));
#21280=CARTESIAN_POINT('Ctrl Pts',(2.56564335337965,4.00344335919148,-11.2011305071679));
#21281=CARTESIAN_POINT('Ctrl Pts',(2.84141117550506,4.06136905899675,-11.3710145555363));
#21282=CARTESIAN_POINT('Ctrl Pts',(3.36597543488952,4.13148157425907,-11.576686812834));
#21283=CARTESIAN_POINT('Ctrl Pts',(3.7087541062761,4.15347422659696,-11.6412306844678));
#21284=CARTESIAN_POINT('Ctrl Pts',(4.,4.15347422659696,-11.6412306844678));
#21285=CARTESIAN_POINT('Ctrl Pts',(4.2912458937239,4.15347422659696,-11.6412306844678));
#21286=CARTESIAN_POINT('Ctrl Pts',(4.63402456511048,4.13148157425907,-11.576686812834));
#21287=CARTESIAN_POINT('Ctrl Pts',(5.15858882449494,4.06136905899675,-11.3710145555363));
#21288=CARTESIAN_POINT('Ctrl Pts',(5.43435664662035,4.00344335919148,-11.2011305071679));
#21289=CARTESIAN_POINT('Ctrl Pts',(5.63694838037123,3.94043853820962,-11.0164851076281));
#21290=CARTESIAN_POINT('Origin',(1.18152580981438,0.,0.));
#21291=CARTESIAN_POINT('',(2.36305161962877,2.83826704815897,-7.79963077096185));
#21292=CARTESIAN_POINT('Origin',(2.36305161962877,0.,0.));
#21293=CARTESIAN_POINT('',(2.36305161962877,2.28830166396292,-7.97832535653345));
#21294=CARTESIAN_POINT('Ctrl Pts',(2.36305161962877,2.83826704815897,-7.79963077096185));
#21295=CARTESIAN_POINT('Ctrl Pts',(2.3422623536685,2.7464656808039,-7.83303706974588));
#21296=CARTESIAN_POINT('Ctrl Pts',(2.33256137669178,2.65313425633026,-7.86508088454567));
#21297=CARTESIAN_POINT('Ctrl Pts',(2.33256137669178,2.47654785029387,-7.92245728595388));
#21298=CARTESIAN_POINT('Ctrl Pts',(2.3422623536685,2.38220626001896,-7.95139213009729));
#21299=CARTESIAN_POINT('Ctrl Pts',(2.36305161962877,2.28830166396292,-7.97832535653345));
#21300=CARTESIAN_POINT('',(2.36305161962877,-2.28830166396292,-7.97832535653345));
#21301=CARTESIAN_POINT('Origin',(2.36305161962877,0.,0.));
#21302=CARTESIAN_POINT('',(2.36305161962877,-2.83826704815898,-7.79963077096185));
#21303=CARTESIAN_POINT('Ctrl Pts',(2.36305161962877,-2.28830166396292,-7.97832535653345));
#21304=CARTESIAN_POINT('Ctrl Pts',(2.3422623536685,-2.38220626001896,-7.95139213009729));
#21305=CARTESIAN_POINT('Ctrl Pts',(2.33256137669178,-2.47654785029387,-7.92245728595388));
#21306=CARTESIAN_POINT('Ctrl Pts',(2.33256137669178,-2.65313425633026,-7.86508088454567));
#21307=CARTESIAN_POINT('Ctrl Pts',(2.3422623536685,-2.7464656808039,-7.83303706974588));
#21308=CARTESIAN_POINT('Ctrl Pts',(2.36305161962877,-2.83826704815898,-7.79963077096185));
#21309=CARTESIAN_POINT('',(2.36305161962877,-6.54081691696392,-5.10957082921439));
#21310=CARTESIAN_POINT('Origin',(2.36305161962877,0.,0.));
#21311=CARTESIAN_POINT('',(2.36305161962877,-6.88071421703298,-4.64174233058237));
#21312=CARTESIAN_POINT('Ctrl Pts',(2.36305161962877,-6.54081691696392,-5.10957082921439));
#21313=CARTESIAN_POINT('Ctrl Pts',(2.3422623536685,-6.60095637772735,-5.03258565462997));
#21314=CARTESIAN_POINT('Ctrl Pts',(2.33256137669179,-6.66027285287123,-4.95372427854694));
#21315=CARTESIAN_POINT('Ctrl Pts',(2.33256137669178,-6.7694092537529,-4.80351090950811));
#21316=CARTESIAN_POINT('Ctrl Pts',(2.3422623536685,-6.82608108049479,-4.72272808388942));
#21317=CARTESIAN_POINT('Ctrl Pts',(2.36305161962877,-6.88071421703298,-4.64174233058237));
#21318=CARTESIAN_POINT('',(2.36305161962877,-8.294962421875,-0.289133913060418));
#21319=CARTESIAN_POINT('Origin',(2.36305161962877,0.,0.));
#21320=CARTESIAN_POINT('',(2.33256137669178,-8.3,-1.01563503836937E-15));
#21321=CARTESIAN_POINT('Ctrl Pts',(2.36305161962877,-8.294962421875,-0.289133913060418));
#21322=CARTESIAN_POINT('Ctrl Pts',(2.3422623536685,-8.29836551739928,-0.191502510389135));
#21323=CARTESIAN_POINT('Ctrl Pts',(2.33256137669178,-8.3,-0.0928369676306304));
#21324=CARTESIAN_POINT('Ctrl Pts',(2.33256137669178,-8.3,-1.01481323344643E-15));
#21325=CARTESIAN_POINT('',(0.,-8.3,-1.0164568432923E-15));
#21326=CARTESIAN_POINT('',(1.18152580981438,-8.3,-1.0164568432923E-15));
#21327=CARTESIAN_POINT('Origin',(0.,0.,0.));
#21328=CARTESIAN_POINT('',(2.36305161962877,-8.294962421875,0.28913391306042));
#21329=CARTESIAN_POINT('Ctrl Pts',(2.33256137669178,-8.3,-1.01481323344643E-15));
#21330=CARTESIAN_POINT('Ctrl Pts',(2.33256137669178,-8.3,0.0928369676306297));
#21331=CARTESIAN_POINT('Ctrl Pts',(2.3422623536685,-8.29836551739928,0.191502510389136));
#21332=CARTESIAN_POINT('Ctrl Pts',(2.36305161962877,-8.294962421875,0.28913391306042));
#21333=CARTESIAN_POINT('',(2.36305161962877,-6.88071421703297,4.64174233058237));
#21334=CARTESIAN_POINT('Origin',(2.36305161962877,0.,0.));
#21335=CARTESIAN_POINT('',(2.36305161962877,-6.54081691696392,5.10957082921439));
#21336=CARTESIAN_POINT('Ctrl Pts',(2.36305161962877,-6.88071421703297,4.64174233058237));
#21337=CARTESIAN_POINT('Ctrl Pts',(2.3422623536685,-6.82608108049479,4.72272808388942));
#21338=CARTESIAN_POINT('Ctrl Pts',(2.33256137669178,-6.7694092537529,4.80351090950811));
#21339=CARTESIAN_POINT('Ctrl Pts',(2.33256137669178,-6.66027285287123,4.95372427854694));
#21340=CARTESIAN_POINT('Ctrl Pts',(2.3422623536685,-6.60095637772735,5.03258565462997));
#21341=CARTESIAN_POINT('Ctrl Pts',(2.36305161962877,-6.54081691696392,5.10957082921439));
#21342=CARTESIAN_POINT('',(2.36305161962877,-2.83826704815897,7.79963077096185));
#21343=CARTESIAN_POINT('Origin',(2.36305161962877,0.,0.));
#21344=CARTESIAN_POINT('',(2.36305161962877,-2.28830166396292,7.97832535653345));
#21345=CARTESIAN_POINT('Ctrl Pts',(2.36305161962877,-2.83826704815897,7.79963077096185));
#21346=CARTESIAN_POINT('Ctrl Pts',(2.3422623536685,-2.7464656808039,7.83303706974588));
#21347=CARTESIAN_POINT('Ctrl Pts',(2.33256137669178,-2.65313425633026,7.86508088454567));
#21348=CARTESIAN_POINT('Ctrl Pts',(2.33256137669178,-2.47654785029387,7.92245728595388));
#21349=CARTESIAN_POINT('Ctrl Pts',(2.3422623536685,-2.38220626001896,7.95139213009729));
#21350=CARTESIAN_POINT('Ctrl Pts',(2.36305161962877,-2.28830166396292,7.97832535653345));
#21351=CARTESIAN_POINT('',(2.36305161962877,2.28830166396292,7.97832535653345));
#21352=CARTESIAN_POINT('Origin',(2.36305161962877,0.,0.));
#21353=CARTESIAN_POINT('',(2.36305161962877,2.83826704815898,7.79963077096185));
#21354=CARTESIAN_POINT('Ctrl Pts',(2.36305161962877,2.28830166396292,7.97832535653344));
#21355=CARTESIAN_POINT('Ctrl Pts',(2.3422623536685,2.38220626001896,7.95139213009729));
#21356=CARTESIAN_POINT('Ctrl Pts',(2.33256137669178,2.47654785029387,7.92245728595388));
#21357=CARTESIAN_POINT('Ctrl Pts',(2.33256137669178,2.65313425633026,7.86508088454567));
#21358=CARTESIAN_POINT('Ctrl Pts',(2.3422623536685,2.7464656808039,7.83303706974588));
#21359=CARTESIAN_POINT('Ctrl Pts',(2.36305161962877,2.83826704815897,7.79963077096185));
#21360=CARTESIAN_POINT('',(2.36305161962877,6.54081691696392,5.10957082921439));
#21361=CARTESIAN_POINT('Origin',(2.36305161962877,0.,0.));
#21362=CARTESIAN_POINT('',(2.36305161962877,6.88071421703298,4.64174233058237));
#21363=CARTESIAN_POINT('Ctrl Pts',(2.36305161962877,6.54081691696392,5.10957082921439));
#21364=CARTESIAN_POINT('Ctrl Pts',(2.3422623536685,6.60095637772735,5.03258565462997));
#21365=CARTESIAN_POINT('Ctrl Pts',(2.33256137669178,6.66027285287123,4.95372427854694));
#21366=CARTESIAN_POINT('Ctrl Pts',(2.33256137669178,6.7694092537529,4.80351090950811));
#21367=CARTESIAN_POINT('Ctrl Pts',(2.3422623536685,6.82608108049479,4.72272808388942));
#21368=CARTESIAN_POINT('Ctrl Pts',(2.36305161962877,6.88071421703298,4.64174233058237));
#21369=CARTESIAN_POINT('',(2.36305161962877,8.294962421875,0.289133913060419));
#21370=CARTESIAN_POINT('Origin',(2.36305161962877,0.,0.));
#21371=CARTESIAN_POINT('',(2.36305161962877,8.294962421875,-0.289133913060419));
#21372=CARTESIAN_POINT('Ctrl Pts',(2.36305161962877,8.294962421875,0.289133913060419));
#21373=CARTESIAN_POINT('Ctrl Pts',(2.3422623536685,8.29836551739928,0.191502510389135));
#21374=CARTESIAN_POINT('Ctrl Pts',(2.33256137669178,8.3,0.0928369676306301));
#21375=CARTESIAN_POINT('Ctrl Pts',(2.33256137669178,8.3,-0.09283696763063));
#21376=CARTESIAN_POINT('Ctrl Pts',(2.3422623536685,8.29836551739928,-0.191502510389135));
#21377=CARTESIAN_POINT('Ctrl Pts',(2.36305161962877,8.294962421875,-0.289133913060419));
#21378=CARTESIAN_POINT('Origin',(2.36305161962877,0.,0.));
#21379=CARTESIAN_POINT('Origin',(4.,0.,0.));
#21380=CARTESIAN_POINT('',(5.63694838037123,2.83826704815896,-7.79963077096186));
#21381=CARTESIAN_POINT('Origin',(5.63694838037123,0.,0.));
#21382=CARTESIAN_POINT('Ctrl Pts',(5.63694838037123,2.83826704815898,-7.79963077096185));
#21383=CARTESIAN_POINT('Ctrl Pts',(5.43435502838932,2.77475170678766,-7.61514961115077));
#21384=CARTESIAN_POINT('Ctrl Pts',(5.1585814386757,2.71625203654638,-7.44544836653197));
#21385=CARTESIAN_POINT('Ctrl Pts',(4.63401515068219,2.64540317647514,-7.24001881570869));
#21386=CARTESIAN_POINT('Ctrl Pts',(4.29124189438349,2.6231528858578,-7.17556053123489));
#21387=CARTESIAN_POINT('Ctrl Pts',(3.70875810561651,2.6231528858578,-7.17556053123489));
#21388=CARTESIAN_POINT('Ctrl Pts',(3.36598484931781,2.64540317647514,-7.24001881570869));
#21389=CARTESIAN_POINT('Ctrl Pts',(2.8414185613243,2.71625203654638,-7.44544836653197));
#21390=CARTESIAN_POINT('Ctrl Pts',(2.56564497161068,2.77475170678765,-7.61514961115078));
#21391=CARTESIAN_POINT('Ctrl Pts',(2.36305161962877,2.83826704815898,-7.79963077096185));
#21392=CARTESIAN_POINT('Origin',(4.,3.09016994374947,-9.51056516295154));
#21393=CARTESIAN_POINT('',(4.,5.35487327317731,-8.77471844509619));
#21394=CARTESIAN_POINT('',(4.,0.825466614321638,-10.2464118808069));
#21395=CARTESIAN_POINT('Origin',(4.,3.09016994374947,-9.51056516295154));
#21396=CARTESIAN_POINT('',(2.36305161962877,3.28744573566193,-11.2286553306742));
#21397=CARTESIAN_POINT('Ctrl Pts',(2.36305161962876,3.28744573566193,-11.2286553306742));
#21398=CARTESIAN_POINT('Ctrl Pts',(2.34215062955512,3.39935280476416,-11.1958919760002));
#21399=CARTESIAN_POINT('Ctrl Pts',(2.33256137669178,3.51096249710822,-11.1613271555422));
#21400=CARTESIAN_POINT('Ctrl Pts',(2.33256137669178,3.72003517126555,-11.0933953257644));
#21401=CARTESIAN_POINT('Ctrl Pts',(2.34215062955513,3.83064600082223,-11.0557563217497));
#21402=CARTESIAN_POINT('Ctrl Pts',(2.36305161962877,3.94043853820961,-11.0164851076281));
#21403=CARTESIAN_POINT('Ctrl Pts',(5.63694838037123,3.28744573566191,-11.2286553306742));
#21404=CARTESIAN_POINT('Ctrl Pts',(5.43435664662035,3.34500560751313,-11.4150699014315));
#21405=CARTESIAN_POINT('Ctrl Pts',(5.15858882449494,3.3979980701903,-11.586556855709));
#21406=CARTESIAN_POINT('Ctrl Pts',(4.63402456511048,3.46216697347001,-11.7941603096066));
#21407=CARTESIAN_POINT('Ctrl Pts',(4.2912458937239,3.4823124798495,-11.8593043553441));
#21408=CARTESIAN_POINT('Ctrl Pts',(4.,3.4823124798495,-11.8593043553441));
#21409=CARTESIAN_POINT('Ctrl Pts',(3.7087541062761,3.4823124798495,-11.8593043553441));
#21410=CARTESIAN_POINT('Ctrl Pts',(3.36597543488952,3.46216697347001,-11.7941603096066));
#21411=CARTESIAN_POINT('Ctrl Pts',(2.84141117550506,3.3979980701903,-11.586556855709));
#21412=CARTESIAN_POINT('Ctrl Pts',(2.56564335337965,3.34500560751313,-11.4150699014315));
#21413=CARTESIAN_POINT('Ctrl Pts',(2.36305161962877,3.28744573566191,-11.2286553306742));
#21414=CARTESIAN_POINT('',(5.63694838037123,2.28830166396294,-7.97832535653344));
#21415=CARTESIAN_POINT('Ctrl Pts',(5.63694838037124,2.28830166396294,-7.97832535653344));
#21416=CARTESIAN_POINT('Ctrl Pts',(5.6577376463315,2.38220626001897,-7.95139213009729));
#21417=CARTESIAN_POINT('Ctrl Pts',(5.66743862330822,2.47654785029387,-7.92245728595388));
#21418=CARTESIAN_POINT('Ctrl Pts',(5.66743862330822,2.65313425633025,-7.86508088454568));
#21419=CARTESIAN_POINT('Ctrl Pts',(5.6577376463315,2.74646568080388,-7.83303706974588));
#21420=CARTESIAN_POINT('Ctrl Pts',(5.63694838037124,2.83826704815896,-7.79963077096186));
#21421=CARTESIAN_POINT('Ctrl Pts',(2.36305161962877,2.28830166396291,-7.97832535653345));
#21422=CARTESIAN_POINT('Ctrl Pts',(2.56564497161068,2.23125134947308,-7.7917435821519));
#21423=CARTESIAN_POINT('Ctrl Pts',(2.8414185613243,2.17883068798099,-7.62006714785691));
#21424=CARTESIAN_POINT('Ctrl Pts',(3.36598484931781,2.11540015945172,-7.41222723500246));
#21425=CARTESIAN_POINT('Ctrl Pts',(3.70875810561651,2.09551339368916,-7.34700099475081));
#21426=CARTESIAN_POINT('Ctrl Pts',(4.29124189438349,2.09551339368916,-7.34700099475081));
#21427=CARTESIAN_POINT('Ctrl Pts',(4.63401515068219,2.11540015945172,-7.41222723500246));
#21428=CARTESIAN_POINT('Ctrl Pts',(5.1585814386757,2.17883068798099,-7.62006714785691));
#21429=CARTESIAN_POINT('Ctrl Pts',(5.43435502838932,2.23125134947308,-7.7917435821519));
#21430=CARTESIAN_POINT('Ctrl Pts',(5.63694838037123,2.28830166396291,-7.97832535653345));
#21431=CARTESIAN_POINT('Origin',(4.,0.,0.));
#21432=CARTESIAN_POINT('',(2.36305161962877,-3.28744573566193,-11.2286553306742));
#21433=CARTESIAN_POINT('Origin',(2.36305161962877,0.,0.));
#21434=CARTESIAN_POINT('Ctrl Pts',(2.36305161962877,-3.28744573566191,-11.2286553306742));
#21435=CARTESIAN_POINT('Ctrl Pts',(2.56564335337965,-3.34500560751313,-11.4150699014315));
#21436=CARTESIAN_POINT('Ctrl Pts',(2.84141117550506,-3.39799807019031,-11.586556855709));
#21437=CARTESIAN_POINT('Ctrl Pts',(3.36597543488952,-3.46216697347002,-11.7941603096066));
#21438=CARTESIAN_POINT('Ctrl Pts',(3.7087541062761,-3.48231247984951,-11.8593043553441));
#21439=CARTESIAN_POINT('Ctrl Pts',(4.,-3.48231247984951,-11.8593043553441));
#21440=CARTESIAN_POINT('Ctrl Pts',(4.2912458937239,-3.48231247984951,-11.8593043553441));
#21441=CARTESIAN_POINT('Ctrl Pts',(4.63402456511049,-3.46216697347002,-11.7941603096066));
#21442=CARTESIAN_POINT('Ctrl Pts',(5.15858882449494,-3.39799807019031,-11.586556855709));
#21443=CARTESIAN_POINT('Ctrl Pts',(5.43435664662035,-3.34500560751314,-11.4150699014315));
#21444=CARTESIAN_POINT('Ctrl Pts',(5.63694838037123,-3.28744573566191,-11.2286553306742));
#21445=CARTESIAN_POINT('Origin',(4.,0.,0.));
#21446=CARTESIAN_POINT('',(5.63694838037123,-2.28830166396294,-7.97832535653344));
#21447=CARTESIAN_POINT('Origin',(5.63694838037123,0.,0.));
#21448=CARTESIAN_POINT('Ctrl Pts',(5.63694838037123,-2.28830166396291,-7.97832535653345));
#21449=CARTESIAN_POINT('Ctrl Pts',(5.43435502838932,-2.23125134947308,-7.7917435821519));
#21450=CARTESIAN_POINT('Ctrl Pts',(5.1585814386757,-2.17883068798099,-7.62006714785691));
#21451=CARTESIAN_POINT('Ctrl Pts',(4.6340151506822,-2.11540015945172,-7.41222723500246));
#21452=CARTESIAN_POINT('Ctrl Pts',(4.29124189438349,-2.09551339368916,-7.34700099475081));
#21453=CARTESIAN_POINT('Ctrl Pts',(3.70875810561651,-2.09551339368916,-7.34700099475081));
#21454=CARTESIAN_POINT('Ctrl Pts',(3.36598484931781,-2.11540015945172,-7.41222723500246));
#21455=CARTESIAN_POINT('Ctrl Pts',(2.8414185613243,-2.17883068798099,-7.62006714785691));
#21456=CARTESIAN_POINT('Ctrl Pts',(2.56564497161068,-2.23125134947308,-7.7917435821519));
#21457=CARTESIAN_POINT('Ctrl Pts',(2.36305161962877,-2.28830166396292,-7.97832535653345));
#21458=CARTESIAN_POINT('Origin',(4.,-3.09016994374948,-9.51056516295153));
#21459=CARTESIAN_POINT('',(4.,-0.825466614321642,-10.2464118808069));
#21460=CARTESIAN_POINT('',(4.,-5.35487327317731,-8.77471844509619));
#21461=CARTESIAN_POINT('Origin',(4.,-3.09016994374948,-9.51056516295153));
#21462=CARTESIAN_POINT('',(2.36305161962877,-3.94043853820961,-11.0164851076281));
#21463=CARTESIAN_POINT('Ctrl Pts',(2.36305161962877,-3.94043853820961,-11.0164851076281));
#21464=CARTESIAN_POINT('Ctrl Pts',(2.34215062955513,-3.83064600082223,-11.0557563217497));
#21465=CARTESIAN_POINT('Ctrl Pts',(2.33256137669178,-3.72003517126555,-11.0933953257644));
#21466=CARTESIAN_POINT('Ctrl Pts',(2.33256137669178,-3.51096249710823,-11.1613271555422));
#21467=CARTESIAN_POINT('Ctrl Pts',(2.34215062955513,-3.39935280476416,-11.1958919760002));
#21468=CARTESIAN_POINT('Ctrl Pts',(2.36305161962877,-3.28744573566193,-11.2286553306742));
#21469=CARTESIAN_POINT('Ctrl Pts',(5.63694838037123,-3.94043853820963,-11.0164851076281));
#21470=CARTESIAN_POINT('Ctrl Pts',(5.43435664662035,-4.00344335919149,-11.2011305071679));
#21471=CARTESIAN_POINT('Ctrl Pts',(5.15858882449494,-4.06136905899675,-11.3710145555363));
#21472=CARTESIAN_POINT('Ctrl Pts',(4.63402456511049,-4.13148157425907,-11.576686812834));
#21473=CARTESIAN_POINT('Ctrl Pts',(4.2912458937239,-4.15347422659696,-11.6412306844678));
#21474=CARTESIAN_POINT('Ctrl Pts',(4.,-4.15347422659696,-11.6412306844678));
#21475=CARTESIAN_POINT('Ctrl Pts',(3.7087541062761,-4.15347422659696,-11.6412306844678));
#21476=CARTESIAN_POINT('Ctrl Pts',(3.36597543488952,-4.13148157425907,-11.576686812834));
#21477=CARTESIAN_POINT('Ctrl Pts',(2.84141117550506,-4.06136905899675,-11.3710145555363));
#21478=CARTESIAN_POINT('Ctrl Pts',(2.56564335337965,-4.00344335919149,-11.2011305071679));
#21479=CARTESIAN_POINT('Ctrl Pts',(2.36305161962877,-3.94043853820963,-11.0164851076281));
#21480=CARTESIAN_POINT('',(5.63694838037123,-2.83826704815896,-7.79963077096186));
#21481=CARTESIAN_POINT('Ctrl Pts',(5.63694838037124,-2.83826704815896,-7.79963077096186));
#21482=CARTESIAN_POINT('Ctrl Pts',(5.6577376463315,-2.74646568080389,-7.83303706974588));
#21483=CARTESIAN_POINT('Ctrl Pts',(5.66743862330822,-2.65313425633025,-7.86508088454567));
#21484=CARTESIAN_POINT('Ctrl Pts',(5.66743862330822,-2.47654785029388,-7.92245728595387));
#21485=CARTESIAN_POINT('Ctrl Pts',(5.6577376463315,-2.38220626001897,-7.95139213009729));
#21486=CARTESIAN_POINT('Ctrl Pts',(5.63694838037124,-2.28830166396294,-7.97832535653344));
#21487=CARTESIAN_POINT('Ctrl Pts',(2.36305161962877,-2.83826704815898,-7.79963077096185));
#21488=CARTESIAN_POINT('Ctrl Pts',(2.56564497161068,-2.77475170678766,-7.61514961115077));
#21489=CARTESIAN_POINT('Ctrl Pts',(2.8414185613243,-2.71625203654638,-7.44544836653197));
#21490=CARTESIAN_POINT('Ctrl Pts',(3.36598484931781,-2.64540317647514,-7.24001881570868));
#21491=CARTESIAN_POINT('Ctrl Pts',(3.70875810561651,-2.6231528858578,-7.17556053123489));
#21492=CARTESIAN_POINT('Ctrl Pts',(4.29124189438349,-2.6231528858578,-7.17556053123489));
#21493=CARTESIAN_POINT('Ctrl Pts',(4.63401515068219,-2.64540317647514,-7.24001881570868));
#21494=CARTESIAN_POINT('Ctrl Pts',(5.1585814386757,-2.71625203654638,-7.44544836653197));
#21495=CARTESIAN_POINT('Ctrl Pts',(5.43435502838932,-2.77475170678766,-7.61514961115077));
#21496=CARTESIAN_POINT('Ctrl Pts',(5.63694838037123,-2.83826704815898,-7.79963077096185));
#21497=CARTESIAN_POINT('Origin',(4.,0.,0.));
#21498=CARTESIAN_POINT('',(2.36305161962877,-9.25963747468151,-7.15186086536041));
#21499=CARTESIAN_POINT('Origin',(2.36305161962877,0.,0.));
#21500=CARTESIAN_POINT('Ctrl Pts',(2.36305161962877,-9.25963747468149,-7.15186086536043));
#21501=CARTESIAN_POINT('Ctrl Pts',(2.56564335337965,-9.41577612470672,-7.26884057730417));
#21502=CARTESIAN_POINT('Ctrl Pts',(2.84141117550506,-9.55944543027122,-7.37642824958397));
#21503=CARTESIAN_POINT('Ctrl Pts',(3.36597543488952,-9.73338541206091,-7.5066654368745));
#21504=CARTESIAN_POINT('Ctrl Pts',(3.7087541062761,-9.7879741784414,-7.54752684540867));
#21505=CARTESIAN_POINT('Ctrl Pts',(4.,-9.7879741784414,-7.54752684540867));
#21506=CARTESIAN_POINT('Ctrl Pts',(4.2912458937239,-9.7879741784414,-7.54752684540867));
#21507=CARTESIAN_POINT('Ctrl Pts',(4.63402456511048,-9.73338541206091,-7.5066654368745));
#21508=CARTESIAN_POINT('Ctrl Pts',(5.15858882449494,-9.55944543027122,-7.37642824958397));
#21509=CARTESIAN_POINT('Ctrl Pts',(5.43435664662035,-9.41577612470672,-7.26884057730417));
#21510=CARTESIAN_POINT('Ctrl Pts',(5.63694838037123,-9.2596374746815,-7.15186086536043));
#21511=CARTESIAN_POINT('Origin',(4.,0.,0.));
#21512=CARTESIAN_POINT('',(5.63694838037123,-6.54081691696393,-5.10957082921437));
#21513=CARTESIAN_POINT('Origin',(5.63694838037123,0.,0.));
#21514=CARTESIAN_POINT('Ctrl Pts',(5.63694838037123,-6.54081691696392,-5.10957082921439));
#21515=CARTESIAN_POINT('Ctrl Pts',(5.43435502838932,-6.38499222767917,-4.99215633639485));
#21516=CARTESIAN_POINT('Ctrl Pts',(5.1585814386757,-6.24167414543093,-4.884079275257));
#21517=CARTESIAN_POINT('Ctrl Pts',(4.63401515068219,-6.06819253427497,-4.75321678286296));
#21518=CARTESIAN_POINT('Ctrl Pts',(4.29124189438349,-6.01376478072751,-4.7121367936512));
#21519=CARTESIAN_POINT('Ctrl Pts',(3.70875810561651,-6.01376478072751,-4.7121367936512));
#21520=CARTESIAN_POINT('Ctrl Pts',(3.36598484931781,-6.06819253427498,-4.75321678286295));
#21521=CARTESIAN_POINT('Ctrl Pts',(2.8414185613243,-6.24167414543094,-4.88407927525699));
#21522=CARTESIAN_POINT('Ctrl Pts',(2.56564497161068,-6.38499222767918,-4.99215633639486));
#21523=CARTESIAN_POINT('Ctrl Pts',(2.36305161962877,-6.54081691696392,-5.10957082921439));
#21524=CARTESIAN_POINT('Origin',(4.,-8.09016994374948,-5.87785252292473));
#21525=CARTESIAN_POINT('',(4.,-6.69050631172802,-7.80432424078007));
#21526=CARTESIAN_POINT('',(4.,-9.48983357577093,-3.95138080506939));
#21527=CARTESIAN_POINT('Origin',(4.,-8.09016994374948,-5.87785252292473));
#21528=CARTESIAN_POINT('',(2.36305161962877,-9.66320922106503,-6.59639201002516));
#21529=CARTESIAN_POINT('Ctrl Pts',(2.36305161962876,-9.66320922106503,-6.59639201002516));
#21530=CARTESIAN_POINT('Ctrl Pts',(2.34215062955512,-9.59746823296338,-6.69269752392734));
#21531=CARTESIAN_POINT('Ctrl Pts',(2.33256137669178,-9.53010584356091,-6.78816353218381));
#21532=CARTESIAN_POINT('Ctrl Pts',(2.33256137669178,-9.40089182481285,-6.96601137146006));
#21533=CARTESIAN_POINT('Ctrl Pts',(2.34215062955512,-9.33091437868292,-7.05957742979088));
#21534=CARTESIAN_POINT('Ctrl Pts',(2.36305161962876,-9.25963747468151,-7.15186086536041));
#21535=CARTESIAN_POINT('Ctrl Pts',(5.63694838037123,-9.66320922106504,-6.59639201002514));
#21536=CARTESIAN_POINT('Ctrl Pts',(5.43435664662035,-9.82271303472002,-6.70873997158946));
#21537=CARTESIAN_POINT('Ctrl Pts',(5.15858882449494,-9.96943124850423,-6.81213118171847));
#21538=CARTESIAN_POINT('Ctrl Pts',(4.63402456511048,-10.1470445845151,-6.93731243067146));
#21539=CARTESIAN_POINT('Ctrl Pts',(4.2912458937239,-10.2027749498801,-6.97660256300298));
#21540=CARTESIAN_POINT('Ctrl Pts',(4.,-10.2027749498801,-6.97660256300298));
#21541=CARTESIAN_POINT('Ctrl Pts',(3.7087541062761,-10.2027749498801,-6.97660256300298));
#21542=CARTESIAN_POINT('Ctrl Pts',(3.36597543488952,-10.1470445845151,-6.93731243067146));
#21543=CARTESIAN_POINT('Ctrl Pts',(2.84141117550507,-9.96943124850423,-6.81213118171847));
#21544=CARTESIAN_POINT('Ctrl Pts',(2.56564335337965,-9.82271303472002,-6.70873997158947));
#21545=CARTESIAN_POINT('Ctrl Pts',(2.36305161962877,-9.66320922106504,-6.59639201002514));
#21546=CARTESIAN_POINT('',(5.63694838037123,-6.88071421703297,-4.64174233058239));
#21547=CARTESIAN_POINT('Ctrl Pts',(5.63694838037124,-6.88071421703297,-4.64174233058239));
#21548=CARTESIAN_POINT('Ctrl Pts',(5.6577376463315,-6.82608108049478,-4.72272808388943));
#21549=CARTESIAN_POINT('Ctrl Pts',(5.66743862330822,-6.7694092537529,-4.80351090950812));
#21550=CARTESIAN_POINT('Ctrl Pts',(5.66743862330822,-6.66027285287123,-4.95372427854694));
#21551=CARTESIAN_POINT('Ctrl Pts',(5.6577376463315,-6.60095637772736,-5.03258565462996));
#21552=CARTESIAN_POINT('Ctrl Pts',(5.63694838037124,-6.54081691696393,-5.10957082921437));
#21553=CARTESIAN_POINT('Ctrl Pts',(2.36305161962877,-6.88071421703298,-4.64174233058237));
#21554=CARTESIAN_POINT('Ctrl Pts',(2.56564497161068,-6.72089392139729,-4.5298273181056));
#21555=CARTESIAN_POINT('Ctrl Pts',(2.8414185613243,-6.57381880512416,-4.4269213706742));
#21556=CARTESIAN_POINT('Ctrl Pts',(3.36598484931781,-6.39575241293544,-4.30236928800296));
#21557=CARTESIAN_POINT('Ctrl Pts',(3.70875810561651,-6.33986392069446,-4.26329983311949));
#21558=CARTESIAN_POINT('Ctrl Pts',(4.29124189438349,-6.33986392069446,-4.26329983311949));
#21559=CARTESIAN_POINT('Ctrl Pts',(4.63401515068219,-6.39575241293545,-4.30236928800294));
#21560=CARTESIAN_POINT('Ctrl Pts',(5.1585814386757,-6.57381880512417,-4.42692137067418));
#21561=CARTESIAN_POINT('Ctrl Pts',(5.43435502838932,-6.72089392139729,-4.5298273181056));
#21562=CARTESIAN_POINT('Ctrl Pts',(5.63694838037123,-6.88071421703298,-4.64174233058237));
#21563=CARTESIAN_POINT('Origin',(4.,0.,0.));
#21564=CARTESIAN_POINT('',(2.36305161962877,-11.694962421875,-0.343298632289181));
#21565=CARTESIAN_POINT('Origin',(2.36305161962877,0.,0.));
#21566=CARTESIAN_POINT('Ctrl Pts',(2.36305161962877,-11.694962421875,-0.3432986322892));
#21567=CARTESIAN_POINT('Ctrl Pts',(2.56564335337965,-11.8900401927221,-0.34616121145108));
#21568=CARTESIAN_POINT('Ctrl Pts',(2.84141117550506,-12.0695095495884,-0.348754767692782));
#21569=CARTESIAN_POINT('Ctrl Pts',(3.36597543488952,-12.2867814488469,-0.351879509430404));
#21570=CARTESIAN_POINT('Ctrl Pts',(3.7087541062761,-12.354962421875,-0.352850611529358));
#21571=CARTESIAN_POINT('Ctrl Pts',(4.,-12.354962421875,-0.352850611529358));
#21572=CARTESIAN_POINT('Ctrl Pts',(4.2912458937239,-12.354962421875,-0.352850611529358));
#21573=CARTESIAN_POINT('Ctrl Pts',(4.63402456511048,-12.2867814488469,-0.351879509430404));
#21574=CARTESIAN_POINT('Ctrl Pts',(5.15858882449494,-12.0695095495884,-0.348754767692782));
#21575=CARTESIAN_POINT('Ctrl Pts',(5.43435664662035,-11.8900401927221,-0.34616121145108));
#21576=CARTESIAN_POINT('Ctrl Pts',(5.63694838037123,-11.694962421875,-0.343298632289199));
#21577=CARTESIAN_POINT('Origin',(4.,0.,0.));
#21578=CARTESIAN_POINT('',(5.63694838037123,-8.294962421875,-0.289133913060398));
#21579=CARTESIAN_POINT('Origin',(5.63694838037123,0.,0.));
#21580=CARTESIAN_POINT('Ctrl Pts',(5.63694838037123,-8.294962421875,-0.28913391306042));
#21581=CARTESIAN_POINT('Ctrl Pts',(5.43435502838932,-8.09988309281573,-0.285735047288132));
#21582=CARTESIAN_POINT('Ctrl Pts',(5.1585814386757,-7.92041022602772,-0.282539123257846));
#21583=CARTESIAN_POINT('Ctrl Pts',(4.63401515068219,-7.70314161128355,-0.278639075566217));
#21584=CARTESIAN_POINT('Ctrl Pts',(4.29124189438349,-7.634962421875,-0.277396497015791));
#21585=CARTESIAN_POINT('Ctrl Pts',(3.70875810561651,-7.634962421875,-0.277396497015791));
#21586=CARTESIAN_POINT('Ctrl Pts',(3.36598484931781,-7.70314161128355,-0.278639075566217));
#21587=CARTESIAN_POINT('Ctrl Pts',(2.8414185613243,-7.92041022602773,-0.282539123257846));
#21588=CARTESIAN_POINT('Ctrl Pts',(2.56564497161068,-8.09988309281573,-0.285735047288137));
#21589=CARTESIAN_POINT('Ctrl Pts',(2.36305161962877,-8.294962421875,-0.289133913060424));
#21590=CARTESIAN_POINT('Origin',(4.,-10.,1.22464679914735E-15));
#21591=CARTESIAN_POINT('',(4.,-10.,-2.38125));
#21592=CARTESIAN_POINT('',(4.,-10.,2.38125));
#21593=CARTESIAN_POINT('Origin',(4.,-10.,1.22464679914735E-15));
#21594=CARTESIAN_POINT('',(2.36305161962877,-11.694962421875,0.343298632289184));
#21595=CARTESIAN_POINT('',(2.33256137669178,-11.7,-5.72234566300149E-17));
#21596=CARTESIAN_POINT('Ctrl Pts',(2.36305161962876,-11.694962421875,0.343298632289185));
#21597=CARTESIAN_POINT('Ctrl Pts',(2.34215062955512,-11.6983838060599,0.226744251613028));
#21598=CARTESIAN_POINT('Ctrl Pts',(2.33256137669178,-11.7,0.109916009498454));
#21599=CARTESIAN_POINT('Ctrl Pts',(2.33256137669178,-11.7,1.28369537222284E-15));
#21600=CARTESIAN_POINT('Ctrl Pts',(5.63694838037123,-11.694962421875,0.343298632289202));
#21601=CARTESIAN_POINT('Ctrl Pts',(5.43435664662035,-11.8900401927221,0.346161211451083));
#21602=CARTESIAN_POINT('Ctrl Pts',(5.15858882449494,-12.0695095495884,0.348754767692785));
#21603=CARTESIAN_POINT('Ctrl Pts',(4.63402456511048,-12.2867814488469,0.351879509430407));
#21604=CARTESIAN_POINT('Ctrl Pts',(4.2912458937239,-12.354962421875,0.352850611529361));
#21605=CARTESIAN_POINT('Ctrl Pts',(4.,-12.354962421875,0.352850611529361));
#21606=CARTESIAN_POINT('Ctrl Pts',(3.7087541062761,-12.354962421875,0.352850611529361));
#21607=CARTESIAN_POINT('Ctrl Pts',(3.36597543488952,-12.2867814488469,0.351879509430407));
#21608=CARTESIAN_POINT('Ctrl Pts',(2.84141117550506,-12.0695095495884,0.348754767692785));
#21609=CARTESIAN_POINT('Ctrl Pts',(2.56564335337965,-11.8900401927221,0.346161211451082));
#21610=CARTESIAN_POINT('Ctrl Pts',(2.36305161962877,-11.694962421875,0.343298632289202));
#21611=CARTESIAN_POINT('Ctrl Pts',(2.33256137669178,-11.7,1.31838984174237E-15));
#21612=CARTESIAN_POINT('Ctrl Pts',(2.33256137669178,-11.7,-0.109916009498451));
#21613=CARTESIAN_POINT('Ctrl Pts',(2.34215062955512,-11.6983838060599,-0.226744251613025));
#21614=CARTESIAN_POINT('Ctrl Pts',(2.36305161962876,-11.694962421875,-0.343298632289182));
#21615=CARTESIAN_POINT('',(5.63694838037123,-8.294962421875,0.2891339130604));
#21616=CARTESIAN_POINT('',(5.66743862330822,-8.3,-1.0503295078889E-15));
#21617=CARTESIAN_POINT('Ctrl Pts',(5.63694838037124,-8.294962421875,0.289133913060401));
#21618=CARTESIAN_POINT('Ctrl Pts',(5.6577376463315,-8.29836551739928,0.191502510389123));
#21619=CARTESIAN_POINT('Ctrl Pts',(5.66743862330822,-8.3,0.092836967630624));
#21620=CARTESIAN_POINT('Ctrl Pts',(5.66743862330822,-8.3,-1.0842021724855E-15));
#21621=CARTESIAN_POINT('Ctrl Pts',(2.36305161962877,-8.294962421875,0.289133913060426));
#21622=CARTESIAN_POINT('Ctrl Pts',(2.56564497161068,-8.09988309281573,0.285735047288139));
#21623=CARTESIAN_POINT('Ctrl Pts',(2.8414185613243,-7.92041022602773,0.282539123257848));
#21624=CARTESIAN_POINT('Ctrl Pts',(3.36598484931781,-7.70314161128355,0.278639075566219));
#21625=CARTESIAN_POINT('Ctrl Pts',(3.70875810561651,-7.634962421875,0.277396497015793));
#21626=CARTESIAN_POINT('Ctrl Pts',(4.29124189438349,-7.634962421875,0.277396497015793));
#21627=CARTESIAN_POINT('Ctrl Pts',(4.63401515068219,-7.70314161128355,0.278639075566219));
#21628=CARTESIAN_POINT('Ctrl Pts',(5.1585814386757,-7.92041022602772,0.282539123257848));
#21629=CARTESIAN_POINT('Ctrl Pts',(5.43435502838932,-8.09988309281573,0.285735047288134));
#21630=CARTESIAN_POINT('Ctrl Pts',(5.63694838037123,-8.294962421875,0.289133913060422));
#21631=CARTESIAN_POINT('Ctrl Pts',(5.66743862330822,-8.3,-1.0842021724855E-15));
#21632=CARTESIAN_POINT('Ctrl Pts',(5.66743862330822,-8.3,-0.0928369676306247));
#21633=CARTESIAN_POINT('Ctrl Pts',(5.6577376463315,-8.29836551739928,-0.191502510389122));
#21634=CARTESIAN_POINT('Ctrl Pts',(5.63694838037124,-8.294962421875,-0.289133913060399));
#21635=CARTESIAN_POINT('Origin',(4.,0.,0.));
#21636=CARTESIAN_POINT('',(2.36305161962877,-9.66320922106502,6.59639201002516));
#21637=CARTESIAN_POINT('Origin',(2.36305161962877,0.,0.));
#21638=CARTESIAN_POINT('Ctrl Pts',(2.36305161962877,-9.66320922106503,6.59639201002515));
#21639=CARTESIAN_POINT('Ctrl Pts',(2.56564335337965,-9.82271303472001,6.70873997158947));
#21640=CARTESIAN_POINT('Ctrl Pts',(2.84141117550506,-9.96943124850423,6.81213118171848));
#21641=CARTESIAN_POINT('Ctrl Pts',(3.36597543488952,-10.1470445845151,6.93731243067146));
#21642=CARTESIAN_POINT('Ctrl Pts',(3.7087541062761,-10.2027749498801,6.97660256300298));
#21643=CARTESIAN_POINT('Ctrl Pts',(4.,-10.2027749498801,6.97660256300298));
#21644=CARTESIAN_POINT('Ctrl Pts',(4.2912458937239,-10.2027749498801,6.97660256300298));
#21645=CARTESIAN_POINT('Ctrl Pts',(4.63402456511048,-10.1470445845151,6.93731243067146));
#21646=CARTESIAN_POINT('Ctrl Pts',(5.15858882449494,-9.96943124850423,6.81213118171848));
#21647=CARTESIAN_POINT('Ctrl Pts',(5.43435664662035,-9.82271303472001,6.70873997158947));
#21648=CARTESIAN_POINT('Ctrl Pts',(5.63694838037123,-9.66320922106503,6.59639201002515));
#21649=CARTESIAN_POINT('Origin',(4.,0.,0.));
#21650=CARTESIAN_POINT('',(5.63694838037123,-6.88071421703296,4.64174233058239));
#21651=CARTESIAN_POINT('Origin',(5.63694838037123,0.,0.));
#21652=CARTESIAN_POINT('Ctrl Pts',(5.63694838037123,-6.88071421703298,4.64174233058237));
#21653=CARTESIAN_POINT('Ctrl Pts',(5.43435502838932,-6.72089392139729,4.5298273181056));
#21654=CARTESIAN_POINT('Ctrl Pts',(5.1585814386757,-6.57381880512416,4.4269213706742));
#21655=CARTESIAN_POINT('Ctrl Pts',(4.6340151506822,-6.39575241293544,4.30236928800296));
#21656=CARTESIAN_POINT('Ctrl Pts',(4.29124189438349,-6.33986392069446,4.26329983311949));
#21657=CARTESIAN_POINT('Ctrl Pts',(3.70875810561651,-6.33986392069446,4.26329983311949));
#21658=CARTESIAN_POINT('Ctrl Pts',(3.36598484931781,-6.39575241293544,4.30236928800296));
#21659=CARTESIAN_POINT('Ctrl Pts',(2.8414185613243,-6.57381880512416,4.4269213706742));
#21660=CARTESIAN_POINT('Ctrl Pts',(2.56564497161068,-6.72089392139729,4.5298273181056));
#21661=CARTESIAN_POINT('Ctrl Pts',(2.36305161962877,-6.88071421703298,4.64174233058237));
#21662=CARTESIAN_POINT('Origin',(4.,-8.09016994374947,5.87785252292473));
#21663=CARTESIAN_POINT('',(4.,-9.48983357577093,3.95138080506939));
#21664=CARTESIAN_POINT('',(4.,-6.69050631172802,7.80432424078008));
#21665=CARTESIAN_POINT('Origin',(4.,-8.09016994374947,5.87785252292473));
#21666=CARTESIAN_POINT('',(2.36305161962877,-9.25963747468151,7.15186086536042));
#21667=CARTESIAN_POINT('Ctrl Pts',(2.36305161962876,-9.25963747468151,7.15186086536042));
#21668=CARTESIAN_POINT('Ctrl Pts',(2.34215062955512,-9.33091437868292,7.05957742979088));
#21669=CARTESIAN_POINT('Ctrl Pts',(2.33256137669178,-9.40089182481285,6.96601137146006));
#21670=CARTESIAN_POINT('Ctrl Pts',(2.33256137669178,-9.53010584356091,6.78816353218381));
#21671=CARTESIAN_POINT('Ctrl Pts',(2.34215062955513,-9.59746823296338,6.69269752392735));
#21672=CARTESIAN_POINT('Ctrl Pts',(2.36305161962877,-9.66320922106503,6.59639201002516));
#21673=CARTESIAN_POINT('Ctrl Pts',(5.63694838037123,-9.2596374746815,7.15186086536043));
#21674=CARTESIAN_POINT('Ctrl Pts',(5.43435664662035,-9.41577612470673,7.26884057730416));
#21675=CARTESIAN_POINT('Ctrl Pts',(5.15858882449494,-9.55944543027121,7.37642824958397));
#21676=CARTESIAN_POINT('Ctrl Pts',(4.63402456511048,-9.73338541206091,7.5066654368745));
#21677=CARTESIAN_POINT('Ctrl Pts',(4.2912458937239,-9.7879741784414,7.54752684540867));
#21678=CARTESIAN_POINT('Ctrl Pts',(4.,-9.7879741784414,7.54752684540867));
#21679=CARTESIAN_POINT('Ctrl Pts',(3.7087541062761,-9.7879741784414,7.54752684540867));
#21680=CARTESIAN_POINT('Ctrl Pts',(3.36597543488952,-9.73338541206091,7.5066654368745));
#21681=CARTESIAN_POINT('Ctrl Pts',(2.84141117550507,-9.55944543027121,7.37642824958397));
#21682=CARTESIAN_POINT('Ctrl Pts',(2.56564335337965,-9.41577612470673,7.26884057730416));
#21683=CARTESIAN_POINT('Ctrl Pts',(2.36305161962877,-9.2596374746815,7.15186086536043));
#21684=CARTESIAN_POINT('',(5.63694838037123,-6.54081691696393,5.10957082921437));
#21685=CARTESIAN_POINT('Ctrl Pts',(5.63694838037124,-6.54081691696393,5.10957082921438));
#21686=CARTESIAN_POINT('Ctrl Pts',(5.6577376463315,-6.60095637772735,5.03258565462996));
#21687=CARTESIAN_POINT('Ctrl Pts',(5.66743862330822,-6.66027285287123,4.95372427854694));
#21688=CARTESIAN_POINT('Ctrl Pts',(5.66743862330822,-6.7694092537529,4.80351090950812));
#21689=CARTESIAN_POINT('Ctrl Pts',(5.6577376463315,-6.82608108049478,4.72272808388943));
#21690=CARTESIAN_POINT('Ctrl Pts',(5.63694838037124,-6.88071421703297,4.64174233058239));
#21691=CARTESIAN_POINT('Ctrl Pts',(2.36305161962877,-6.54081691696391,5.10957082921439));
#21692=CARTESIAN_POINT('Ctrl Pts',(2.56564497161068,-6.38499222767917,4.99215633639486));
#21693=CARTESIAN_POINT('Ctrl Pts',(2.8414185613243,-6.24167414543094,4.88407927525699));
#21694=CARTESIAN_POINT('Ctrl Pts',(3.36598484931781,-6.06819253427498,4.75321678286295));
#21695=CARTESIAN_POINT('Ctrl Pts',(3.70875810561651,-6.0137647807275,4.7121367936512));
#21696=CARTESIAN_POINT('Ctrl Pts',(4.29124189438349,-6.0137647807275,4.7121367936512));
#21697=CARTESIAN_POINT('Ctrl Pts',(4.6340151506822,-6.06819253427498,4.75321678286295));
#21698=CARTESIAN_POINT('Ctrl Pts',(5.1585814386757,-6.24167414543094,4.88407927525699));
#21699=CARTESIAN_POINT('Ctrl Pts',(5.43435502838932,-6.38499222767917,4.99215633639486));
#21700=CARTESIAN_POINT('Ctrl Pts',(5.63694838037123,-6.54081691696391,5.10957082921439));
#21701=CARTESIAN_POINT('Origin',(4.,0.,0.));
#21702=CARTESIAN_POINT('',(2.36305161962877,-3.94043853820961,11.0164851076281));
#21703=CARTESIAN_POINT('Origin',(2.36305161962877,0.,0.));
#21704=CARTESIAN_POINT('Ctrl Pts',(2.36305161962877,-3.94043853820963,11.0164851076281));
#21705=CARTESIAN_POINT('Ctrl Pts',(2.56564335337965,-4.00344335919149,11.2011305071679));
#21706=CARTESIAN_POINT('Ctrl Pts',(2.84141117550506,-4.06136905899675,11.3710145555363));
#21707=CARTESIAN_POINT('Ctrl Pts',(3.36597543488952,-4.13148157425907,11.576686812834));
#21708=CARTESIAN_POINT('Ctrl Pts',(3.7087541062761,-4.15347422659696,11.6412306844678));
#21709=CARTESIAN_POINT('Ctrl Pts',(4.,-4.15347422659696,11.6412306844678));
#21710=CARTESIAN_POINT('Ctrl Pts',(4.2912458937239,-4.15347422659696,11.6412306844678));
#21711=CARTESIAN_POINT('Ctrl Pts',(4.63402456511048,-4.13148157425907,11.576686812834));
#21712=CARTESIAN_POINT('Ctrl Pts',(5.15858882449494,-4.06136905899675,11.3710145555363));
#21713=CARTESIAN_POINT('Ctrl Pts',(5.43435664662035,-4.00344335919149,11.2011305071678));
#21714=CARTESIAN_POINT('Ctrl Pts',(5.63694838037123,-3.94043853820963,11.0164851076281));
#21715=CARTESIAN_POINT('Origin',(4.,0.,0.));
#21716=CARTESIAN_POINT('',(5.63694838037123,-2.83826704815896,7.79963077096186));
#21717=CARTESIAN_POINT('Origin',(5.63694838037123,0.,0.));
#21718=CARTESIAN_POINT('Ctrl Pts',(5.63694838037123,-2.83826704815898,7.79963077096185));
#21719=CARTESIAN_POINT('Ctrl Pts',(5.43435502838932,-2.77475170678765,7.61514961115077));
#21720=CARTESIAN_POINT('Ctrl Pts',(5.1585814386757,-2.71625203654638,7.44544836653197));
#21721=CARTESIAN_POINT('Ctrl Pts',(4.63401515068219,-2.64540317647514,7.24001881570869));
#21722=CARTESIAN_POINT('Ctrl Pts',(4.29124189438349,-2.6231528858578,7.17556053123489));
#21723=CARTESIAN_POINT('Ctrl Pts',(3.70875810561651,-2.6231528858578,7.17556053123489));
#21724=CARTESIAN_POINT('Ctrl Pts',(3.36598484931781,-2.64540317647514,7.24001881570869));
#21725=CARTESIAN_POINT('Ctrl Pts',(2.8414185613243,-2.71625203654638,7.44544836653197));
#21726=CARTESIAN_POINT('Ctrl Pts',(2.56564497161068,-2.77475170678766,7.61514961115078));
#21727=CARTESIAN_POINT('Ctrl Pts',(2.36305161962877,-2.83826704815898,7.79963077096185));
#21728=CARTESIAN_POINT('Origin',(4.,-3.09016994374947,9.51056516295154));
#21729=CARTESIAN_POINT('',(4.,-5.35487327317731,8.77471844509619));
#21730=CARTESIAN_POINT('',(4.,-0.82546661432164,10.2464118808069));
#21731=CARTESIAN_POINT('Origin',(4.,-3.09016994374947,9.51056516295154));
#21732=CARTESIAN_POINT('',(2.36305161962877,-3.28744573566193,11.2286553306742));
#21733=CARTESIAN_POINT('Ctrl Pts',(2.36305161962876,-3.28744573566193,11.2286553306742));
#21734=CARTESIAN_POINT('Ctrl Pts',(2.34215062955512,-3.39935280476416,11.1958919760002));
#21735=CARTESIAN_POINT('Ctrl Pts',(2.33256137669178,-3.51096249710822,11.1613271555422));
#21736=CARTESIAN_POINT('Ctrl Pts',(2.33256137669178,-3.72003517126555,11.0933953257644));
#21737=CARTESIAN_POINT('Ctrl Pts',(2.34215062955512,-3.83064600082223,11.0557563217497));
#21738=CARTESIAN_POINT('Ctrl Pts',(2.36305161962876,-3.94043853820961,11.0164851076281));
#21739=CARTESIAN_POINT('Ctrl Pts',(5.63694838037123,-3.28744573566191,11.2286553306742));
#21740=CARTESIAN_POINT('Ctrl Pts',(5.43435664662035,-3.34500560751313,11.4150699014315));
#21741=CARTESIAN_POINT('Ctrl Pts',(5.15858882449494,-3.3979980701903,11.586556855709));
#21742=CARTESIAN_POINT('Ctrl Pts',(4.63402456511048,-3.46216697347001,11.7941603096066));
#21743=CARTESIAN_POINT('Ctrl Pts',(4.2912458937239,-3.4823124798495,11.8593043553441));
#21744=CARTESIAN_POINT('Ctrl Pts',(4.,-3.4823124798495,11.8593043553441));
#21745=CARTESIAN_POINT('Ctrl Pts',(3.7087541062761,-3.4823124798495,11.8593043553441));
#21746=CARTESIAN_POINT('Ctrl Pts',(3.36597543488952,-3.46216697347001,11.7941603096066));
#21747=CARTESIAN_POINT('Ctrl Pts',(2.84141117550506,-3.3979980701903,11.586556855709));
#21748=CARTESIAN_POINT('Ctrl Pts',(2.56564335337965,-3.34500560751314,11.4150699014315));
#21749=CARTESIAN_POINT('Ctrl Pts',(2.36305161962877,-3.28744573566191,11.2286553306742));
#21750=CARTESIAN_POINT('',(5.63694838037123,-2.28830166396294,7.97832535653344));
#21751=CARTESIAN_POINT('Ctrl Pts',(5.63694838037124,-2.28830166396294,7.97832535653344));
#21752=CARTESIAN_POINT('Ctrl Pts',(5.6577376463315,-2.38220626001897,7.95139213009729));
#21753=CARTESIAN_POINT('Ctrl Pts',(5.66743862330822,-2.47654785029387,7.92245728595388));
#21754=CARTESIAN_POINT('Ctrl Pts',(5.66743862330822,-2.65313425633025,7.86508088454568));
#21755=CARTESIAN_POINT('Ctrl Pts',(5.6577376463315,-2.74646568080388,7.83303706974588));
#21756=CARTESIAN_POINT('Ctrl Pts',(5.63694838037124,-2.83826704815896,7.79963077096186));
#21757=CARTESIAN_POINT('Ctrl Pts',(2.36305161962877,-2.28830166396291,7.97832535653345));
#21758=CARTESIAN_POINT('Ctrl Pts',(2.56564497161068,-2.23125134947308,7.7917435821519));
#21759=CARTESIAN_POINT('Ctrl Pts',(2.8414185613243,-2.17883068798099,7.62006714785691));
#21760=CARTESIAN_POINT('Ctrl Pts',(3.36598484931781,-2.11540015945172,7.41222723500246));
#21761=CARTESIAN_POINT('Ctrl Pts',(3.70875810561651,-2.09551339368916,7.34700099475081));
#21762=CARTESIAN_POINT('Ctrl Pts',(4.29124189438349,-2.09551339368916,7.34700099475081));
#21763=CARTESIAN_POINT('Ctrl Pts',(4.63401515068219,-2.11540015945172,7.41222723500246));
#21764=CARTESIAN_POINT('Ctrl Pts',(5.1585814386757,-2.17883068798099,7.62006714785691));
#21765=CARTESIAN_POINT('Ctrl Pts',(5.43435502838932,-2.23125134947309,7.7917435821519));
#21766=CARTESIAN_POINT('Ctrl Pts',(5.63694838037123,-2.28830166396292,7.97832535653345));
#21767=CARTESIAN_POINT('Origin',(4.,0.,0.));
#21768=CARTESIAN_POINT('',(2.36305161962877,3.28744573566193,11.2286553306742));
#21769=CARTESIAN_POINT('Origin',(2.36305161962877,0.,0.));
#21770=CARTESIAN_POINT('Ctrl Pts',(2.36305161962877,3.2874457356619,11.2286553306742));
#21771=CARTESIAN_POINT('Ctrl Pts',(2.56564335337965,3.34500560751313,11.4150699014315));
#21772=CARTESIAN_POINT('Ctrl Pts',(2.84141117550507,3.39799807019037,11.586556855709));
#21773=CARTESIAN_POINT('Ctrl Pts',(3.36597543488952,3.46216697347008,11.7941603096066));
#21774=CARTESIAN_POINT('Ctrl Pts',(3.7087541062761,3.48231247984951,11.8593043553441));
#21775=CARTESIAN_POINT('Ctrl Pts',(4.,3.48231247984951,11.8593043553441));
#21776=CARTESIAN_POINT('Ctrl Pts',(4.2912458937239,3.48231247984951,11.8593043553441));
#21777=CARTESIAN_POINT('Ctrl Pts',(4.63402456511048,3.46216697347008,11.7941603096066));
#21778=CARTESIAN_POINT('Ctrl Pts',(5.15858882449494,3.39799807019037,11.586556855709));
#21779=CARTESIAN_POINT('Ctrl Pts',(5.43435664662035,3.34500560751313,11.4150699014315));
#21780=CARTESIAN_POINT('Ctrl Pts',(5.63694838037123,3.2874457356619,11.2286553306742));
#21781=CARTESIAN_POINT('Origin',(4.,0.,0.));
#21782=CARTESIAN_POINT('',(5.63694838037123,2.28830166396294,7.97832535653344));
#21783=CARTESIAN_POINT('Origin',(5.63694838037123,0.,0.));
#21784=CARTESIAN_POINT('Ctrl Pts',(5.63694838037123,2.28830166396292,7.97832535653345));
#21785=CARTESIAN_POINT('Ctrl Pts',(5.43435502838932,2.23125134947309,7.7917435821519));
#21786=CARTESIAN_POINT('Ctrl Pts',(5.1585814386757,2.17883068798099,7.62006714785691));
#21787=CARTESIAN_POINT('Ctrl Pts',(4.6340151506822,2.11540015945172,7.41222723500246));
#21788=CARTESIAN_POINT('Ctrl Pts',(4.29124189438349,2.09551339368916,7.34700099475081));
#21789=CARTESIAN_POINT('Ctrl Pts',(3.70875810561651,2.09551339368916,7.34700099475081));
#21790=CARTESIAN_POINT('Ctrl Pts',(3.36598484931781,2.11540015945172,7.41222723500246));
#21791=CARTESIAN_POINT('Ctrl Pts',(2.8414185613243,2.17883068798099,7.62006714785691));
#21792=CARTESIAN_POINT('Ctrl Pts',(2.56564497161068,2.23125134947309,7.7917435821519));
#21793=CARTESIAN_POINT('Ctrl Pts',(2.36305161962877,2.28830166396292,7.97832535653345));
#21794=CARTESIAN_POINT('Origin',(4.,3.09016994374947,9.51056516295154));
#21795=CARTESIAN_POINT('',(4.,0.825466614321642,10.2464118808069));
#21796=CARTESIAN_POINT('',(4.,5.35487327317731,8.77471844509619));
#21797=CARTESIAN_POINT('Origin',(4.,3.09016994374947,9.51056516295154));
#21798=CARTESIAN_POINT('',(2.36305161962877,3.94043853820961,11.0164851076281));
#21799=CARTESIAN_POINT('Ctrl Pts',(2.36305161962876,3.94043853820961,11.0164851076281));
#21800=CARTESIAN_POINT('Ctrl Pts',(2.34215062955512,3.83064600082223,11.0557563217497));
#21801=CARTESIAN_POINT('Ctrl Pts',(2.33256137669178,3.72003517126555,11.0933953257644));
#21802=CARTESIAN_POINT('Ctrl Pts',(2.33256137669178,3.51096249710822,11.1613271555422));
#21803=CARTESIAN_POINT('Ctrl Pts',(2.34215062955512,3.39935280476416,11.1958919760002));
#21804=CARTESIAN_POINT('Ctrl Pts',(2.36305161962876,3.28744573566193,11.2286553306742));
#21805=CARTESIAN_POINT('Ctrl Pts',(5.63694838037123,3.94043853820963,11.0164851076281));
#21806=CARTESIAN_POINT('Ctrl Pts',(5.43435664662035,4.00344335919149,11.2011305071679));
#21807=CARTESIAN_POINT('Ctrl Pts',(5.15858882449494,4.06136905899669,11.3710145555363));
#21808=CARTESIAN_POINT('Ctrl Pts',(4.63402456511048,4.13148157425901,11.576686812834));
#21809=CARTESIAN_POINT('Ctrl Pts',(4.2912458937239,4.15347422659696,11.6412306844678));
#21810=CARTESIAN_POINT('Ctrl Pts',(4.,4.15347422659696,11.6412306844678));
#21811=CARTESIAN_POINT('Ctrl Pts',(3.7087541062761,4.15347422659696,11.6412306844678));
#21812=CARTESIAN_POINT('Ctrl Pts',(3.36597543488952,4.13148157425901,11.576686812834));
#21813=CARTESIAN_POINT('Ctrl Pts',(2.84141117550507,4.06136905899669,11.3710145555363));
#21814=CARTESIAN_POINT('Ctrl Pts',(2.56564335337965,4.00344335919149,11.2011305071678));
#21815=CARTESIAN_POINT('Ctrl Pts',(2.36305161962877,3.94043853820963,11.0164851076281));
#21816=CARTESIAN_POINT('',(5.63694838037123,2.83826704815896,7.79963077096186));
#21817=CARTESIAN_POINT('Ctrl Pts',(5.63694838037124,2.83826704815896,7.79963077096186));
#21818=CARTESIAN_POINT('Ctrl Pts',(5.6577376463315,2.74646568080389,7.83303706974588));
#21819=CARTESIAN_POINT('Ctrl Pts',(5.66743862330822,2.65313425633025,7.86508088454568));
#21820=CARTESIAN_POINT('Ctrl Pts',(5.66743862330822,2.47654785029388,7.92245728595387));
#21821=CARTESIAN_POINT('Ctrl Pts',(5.6577376463315,2.38220626001897,7.95139213009729));
#21822=CARTESIAN_POINT('Ctrl Pts',(5.63694838037124,2.28830166396294,7.97832535653344));
#21823=CARTESIAN_POINT('Ctrl Pts',(2.36305161962877,2.83826704815898,7.79963077096185));
#21824=CARTESIAN_POINT('Ctrl Pts',(2.56564497161068,2.77475170678765,7.61514961115078));
#21825=CARTESIAN_POINT('Ctrl Pts',(2.8414185613243,2.71625203654638,7.44544836653197));
#21826=CARTESIAN_POINT('Ctrl Pts',(3.36598484931781,2.64540317647514,7.24001881570869));
#21827=CARTESIAN_POINT('Ctrl Pts',(3.70875810561651,2.6231528858578,7.17556053123489));
#21828=CARTESIAN_POINT('Ctrl Pts',(4.29124189438349,2.6231528858578,7.17556053123489));
#21829=CARTESIAN_POINT('Ctrl Pts',(4.6340151506822,2.64540317647514,7.24001881570869));
#21830=CARTESIAN_POINT('Ctrl Pts',(5.1585814386757,2.71625203654638,7.44544836653197));
#21831=CARTESIAN_POINT('Ctrl Pts',(5.43435502838932,2.77475170678765,7.61514961115077));
#21832=CARTESIAN_POINT('Ctrl Pts',(5.63694838037123,2.83826704815898,7.79963077096185));
#21833=CARTESIAN_POINT('Origin',(4.,0.,0.));
#21834=CARTESIAN_POINT('',(2.36305161962877,9.25963747468151,7.15186086536041));
#21835=CARTESIAN_POINT('Origin',(2.36305161962877,0.,0.));
#21836=CARTESIAN_POINT('Ctrl Pts',(2.36305161962877,9.2596374746815,7.15186086536043));
#21837=CARTESIAN_POINT('Ctrl Pts',(2.56564335337965,9.41577612470673,7.26884057730416));
#21838=CARTESIAN_POINT('Ctrl Pts',(2.84141117550506,9.55944543027122,7.37642824958397));
#21839=CARTESIAN_POINT('Ctrl Pts',(3.36597543488952,9.73338541206091,7.5066654368745));
#21840=CARTESIAN_POINT('Ctrl Pts',(3.7087541062761,9.7879741784414,7.54752684540867));
#21841=CARTESIAN_POINT('Ctrl Pts',(4.,9.7879741784414,7.54752684540867));
#21842=CARTESIAN_POINT('Ctrl Pts',(4.2912458937239,9.7879741784414,7.54752684540867));
#21843=CARTESIAN_POINT('Ctrl Pts',(4.63402456511048,9.73338541206091,7.5066654368745));
#21844=CARTESIAN_POINT('Ctrl Pts',(5.15858882449494,9.55944543027121,7.37642824958397));
#21845=CARTESIAN_POINT('Ctrl Pts',(5.43435664662035,9.41577612470672,7.26884057730416));
#21846=CARTESIAN_POINT('Ctrl Pts',(5.63694838037123,9.2596374746815,7.15186086536043));
#21847=CARTESIAN_POINT('Origin',(4.,0.,0.));
#21848=CARTESIAN_POINT('',(5.63694838037123,6.54081691696393,5.10957082921437));
#21849=CARTESIAN_POINT('Origin',(5.63694838037123,0.,0.));
#21850=CARTESIAN_POINT('Ctrl Pts',(5.63694838037123,6.54081691696392,5.10957082921439));
#21851=CARTESIAN_POINT('Ctrl Pts',(5.43435502838932,6.38499222767917,4.99215633639486));
#21852=CARTESIAN_POINT('Ctrl Pts',(5.1585814386757,6.24167414543094,4.88407927525699));
#21853=CARTESIAN_POINT('Ctrl Pts',(4.63401515068219,6.06819253427498,4.75321678286295));
#21854=CARTESIAN_POINT('Ctrl Pts',(4.29124189438349,6.01376478072751,4.7121367936512));
#21855=CARTESIAN_POINT('Ctrl Pts',(3.70875810561651,6.01376478072751,4.7121367936512));
#21856=CARTESIAN_POINT('Ctrl Pts',(3.36598484931781,6.06819253427498,4.75321678286295));
#21857=CARTESIAN_POINT('Ctrl Pts',(2.8414185613243,6.24167414543094,4.88407927525699));
#21858=CARTESIAN_POINT('Ctrl Pts',(2.56564497161068,6.38499222767917,4.99215633639486));
#21859=CARTESIAN_POINT('Ctrl Pts',(2.36305161962877,6.54081691696392,5.10957082921439));
#21860=CARTESIAN_POINT('Origin',(4.,8.09016994374947,5.87785252292473));
#21861=CARTESIAN_POINT('',(4.,6.69050631172802,7.80432424078007));
#21862=CARTESIAN_POINT('',(4.,9.48983357577093,3.95138080506939));
#21863=CARTESIAN_POINT('Origin',(4.,8.09016994374947,5.87785252292473));
#21864=CARTESIAN_POINT('',(2.36305161962877,9.66320922106503,6.59639201002516));
#21865=CARTESIAN_POINT('Ctrl Pts',(2.36305161962877,9.66320922106503,6.59639201002516));
#21866=CARTESIAN_POINT('Ctrl Pts',(2.34215062955513,9.59746823296338,6.69269752392734));
#21867=CARTESIAN_POINT('Ctrl Pts',(2.33256137669178,9.53010584356091,6.78816353218381));
#21868=CARTESIAN_POINT('Ctrl Pts',(2.33256137669178,9.40089182481286,6.96601137146006));
#21869=CARTESIAN_POINT('Ctrl Pts',(2.34215062955512,9.33091437868292,7.05957742979088));
#21870=CARTESIAN_POINT('Ctrl Pts',(2.36305161962876,9.25963747468151,7.15186086536041));
#21871=CARTESIAN_POINT('Ctrl Pts',(5.63694838037123,9.66320922106504,6.59639201002515));
#21872=CARTESIAN_POINT('Ctrl Pts',(5.43435664662035,9.82271303472001,6.70873997158947));
#21873=CARTESIAN_POINT('Ctrl Pts',(5.15858882449494,9.96943124850423,6.81213118171848));
#21874=CARTESIAN_POINT('Ctrl Pts',(4.63402456511048,10.1470445845151,6.93731243067146));
#21875=CARTESIAN_POINT('Ctrl Pts',(4.2912458937239,10.2027749498801,6.97660256300298));
#21876=CARTESIAN_POINT('Ctrl Pts',(4.,10.2027749498801,6.97660256300298));
#21877=CARTESIAN_POINT('Ctrl Pts',(3.7087541062761,10.2027749498801,6.97660256300298));
#21878=CARTESIAN_POINT('Ctrl Pts',(3.36597543488952,10.1470445845151,6.93731243067146));
#21879=CARTESIAN_POINT('Ctrl Pts',(2.84141117550506,9.96943124850423,6.81213118171847));
#21880=CARTESIAN_POINT('Ctrl Pts',(2.56564335337965,9.82271303472001,6.70873997158947));
#21881=CARTESIAN_POINT('Ctrl Pts',(2.36305161962877,9.66320922106504,6.59639201002515));
#21882=CARTESIAN_POINT('',(5.63694838037123,6.88071421703297,4.64174233058239));
#21883=CARTESIAN_POINT('Ctrl Pts',(5.63694838037124,6.88071421703297,4.64174233058239));
#21884=CARTESIAN_POINT('Ctrl Pts',(5.6577376463315,6.82608108049478,4.72272808388943));
#21885=CARTESIAN_POINT('Ctrl Pts',(5.66743862330822,6.7694092537529,4.80351090950812));
#21886=CARTESIAN_POINT('Ctrl Pts',(5.66743862330822,6.66027285287123,4.95372427854694));
#21887=CARTESIAN_POINT('Ctrl Pts',(5.6577376463315,6.60095637772736,5.03258565462996));
#21888=CARTESIAN_POINT('Ctrl Pts',(5.63694838037124,6.54081691696393,5.10957082921437));
#21889=CARTESIAN_POINT('Ctrl Pts',(2.36305161962877,6.88071421703298,4.64174233058237));
#21890=CARTESIAN_POINT('Ctrl Pts',(2.56564497161068,6.72089392139729,4.5298273181056));
#21891=CARTESIAN_POINT('Ctrl Pts',(2.8414185613243,6.57381880512416,4.4269213706742));
#21892=CARTESIAN_POINT('Ctrl Pts',(3.36598484931781,6.39575241293544,4.30236928800296));
#21893=CARTESIAN_POINT('Ctrl Pts',(3.70875810561651,6.33986392069446,4.26329983311949));
#21894=CARTESIAN_POINT('Ctrl Pts',(4.29124189438349,6.33986392069446,4.26329983311949));
#21895=CARTESIAN_POINT('Ctrl Pts',(4.63401515068219,6.39575241293544,4.30236928800296));
#21896=CARTESIAN_POINT('Ctrl Pts',(5.1585814386757,6.57381880512416,4.4269213706742));
#21897=CARTESIAN_POINT('Ctrl Pts',(5.43435502838932,6.72089392139729,4.5298273181056));
#21898=CARTESIAN_POINT('Ctrl Pts',(5.63694838037123,6.88071421703298,4.64174233058237));
#21899=CARTESIAN_POINT('Origin',(1.18152580981438,0.,0.));
#21900=CARTESIAN_POINT('',(2.36305161962877,11.694962421875,-0.343298632289183));
#21901=CARTESIAN_POINT('Origin',(2.36305161962877,0.,0.));
#21902=CARTESIAN_POINT('',(2.36305161962877,11.694962421875,0.343298632289183));
#21903=CARTESIAN_POINT('Ctrl Pts',(2.36305161962876,11.694962421875,-0.343298632289183));
#21904=CARTESIAN_POINT('Ctrl Pts',(2.34215062955512,11.6983838060599,-0.226744251613026));
#21905=CARTESIAN_POINT('Ctrl Pts',(2.33256137669178,11.7,-0.109916009498452));
#21906=CARTESIAN_POINT('Ctrl Pts',(2.33256137669178,11.7,0.109916009498452));
#21907=CARTESIAN_POINT('Ctrl Pts',(2.34215062955512,11.6983838060599,0.226744251613026));
#21908=CARTESIAN_POINT('Ctrl Pts',(2.36305161962876,11.694962421875,0.343298632289183));
#21909=CARTESIAN_POINT('Origin',(2.36305161962877,0.,0.));
#21910=CARTESIAN_POINT('',(0.,-11.7,-1.4328367550024E-15));
#21911=CARTESIAN_POINT('',(1.18152580981438,-11.7,-1.4328367550024E-15));
#21912=CARTESIAN_POINT('Origin',(0.,0.,0.));
#21913=CARTESIAN_POINT('Origin',(4.,0.,0.));
#21914=CARTESIAN_POINT('Ctrl Pts',(5.63694838037123,11.694962421875,-0.3432986322892));
#21915=CARTESIAN_POINT('Ctrl Pts',(5.43435664662035,11.8900401927221,-0.346161211451081));
#21916=CARTESIAN_POINT('Ctrl Pts',(5.15858882449494,12.0695095495884,-0.348754767692784));
#21917=CARTESIAN_POINT('Ctrl Pts',(4.63402456511048,12.2867814488469,-0.351879509430406));
#21918=CARTESIAN_POINT('Ctrl Pts',(4.2912458937239,12.354962421875,-0.35285061152936));
#21919=CARTESIAN_POINT('Ctrl Pts',(4.,12.354962421875,-0.35285061152936));
#21920=CARTESIAN_POINT('Ctrl Pts',(3.7087541062761,12.354962421875,-0.35285061152936));
#21921=CARTESIAN_POINT('Ctrl Pts',(3.36597543488952,12.2867814488469,-0.351879509430406));
#21922=CARTESIAN_POINT('Ctrl Pts',(2.84141117550506,12.0695095495884,-0.348754767692784));
#21923=CARTESIAN_POINT('Ctrl Pts',(2.56564335337965,11.8900401927221,-0.346161211451081));
#21924=CARTESIAN_POINT('Ctrl Pts',(2.36305161962877,11.694962421875,-0.343298632289201));
#21925=CARTESIAN_POINT('Origin',(6.81847419018562,0.,0.));
#21926=CARTESIAN_POINT('',(8.,-8.3,-1.0164568432923E-15));
#21927=CARTESIAN_POINT('Origin',(8.,0.,0.));
#21928=CARTESIAN_POINT('',(6.81847419018562,-8.3,-1.0164568432923E-15));
#21929=CARTESIAN_POINT('',(5.63694838037123,8.294962421875,-0.289133913060399));
#21930=CARTESIAN_POINT('Origin',(5.63694838037123,0.,0.));
#21931=CARTESIAN_POINT('',(5.63694838037123,8.294962421875,0.289133913060399));
#21932=CARTESIAN_POINT('Ctrl Pts',(5.63694838037124,8.294962421875,-0.2891339130604));
#21933=CARTESIAN_POINT('Ctrl Pts',(5.6577376463315,8.29836551739928,-0.191502510389123));
#21934=CARTESIAN_POINT('Ctrl Pts',(5.66743862330822,8.3,-0.0928369676306243));
#21935=CARTESIAN_POINT('Ctrl Pts',(5.66743862330822,8.3,0.0928369676306244));
#21936=CARTESIAN_POINT('Ctrl Pts',(5.6577376463315,8.29836551739928,0.191502510389123));
#21937=CARTESIAN_POINT('Ctrl Pts',(5.63694838037124,8.294962421875,0.2891339130604));
#21938=CARTESIAN_POINT('Origin',(5.63694838037123,0.,0.));
#21939=CARTESIAN_POINT('Origin',(4.,0.,0.));
#21940=CARTESIAN_POINT('Ctrl Pts',(2.36305161962877,8.294962421875,-0.289133913060425));
#21941=CARTESIAN_POINT('Ctrl Pts',(2.56564497161068,8.09988309281573,-0.285735047288138));
#21942=CARTESIAN_POINT('Ctrl Pts',(2.8414185613243,7.92041022602773,-0.282539123257847));
#21943=CARTESIAN_POINT('Ctrl Pts',(3.36598484931781,7.70314161128355,-0.278639075566218));
#21944=CARTESIAN_POINT('Ctrl Pts',(3.70875810561651,7.634962421875,-0.277396497015792));
#21945=CARTESIAN_POINT('Ctrl Pts',(4.29124189438349,7.634962421875,-0.277396497015792));
#21946=CARTESIAN_POINT('Ctrl Pts',(4.63401515068219,7.70314161128355,-0.278639075566218));
#21947=CARTESIAN_POINT('Ctrl Pts',(5.1585814386757,7.92041022602772,-0.282539123257847));
#21948=CARTESIAN_POINT('Ctrl Pts',(5.43435502838932,8.09988309281573,-0.285735047288133));
#21949=CARTESIAN_POINT('Ctrl Pts',(5.63694838037123,8.294962421875,-0.289133913060422));
#21950=CARTESIAN_POINT('Origin',(4.,10.,0.));
#21951=CARTESIAN_POINT('',(4.,10.,2.38125));
#21952=CARTESIAN_POINT('',(4.,10.,-2.38125));
#21953=CARTESIAN_POINT('Origin',(4.,10.,0.));
#21954=CARTESIAN_POINT('Ctrl Pts',(5.63694838037123,8.294962421875,0.289133913060422));
#21955=CARTESIAN_POINT('Ctrl Pts',(5.43435502838932,8.09988309281573,0.285735047288134));
#21956=CARTESIAN_POINT('Ctrl Pts',(5.1585814386757,7.92041022602772,0.282539123257847));
#21957=CARTESIAN_POINT('Ctrl Pts',(4.63401515068219,7.70314161128355,0.278639075566218));
#21958=CARTESIAN_POINT('Ctrl Pts',(4.29124189438349,7.634962421875,0.277396497015792));
#21959=CARTESIAN_POINT('Ctrl Pts',(3.70875810561651,7.634962421875,0.277396497015792));
#21960=CARTESIAN_POINT('Ctrl Pts',(3.36598484931781,7.70314161128355,0.278639075566218));
#21961=CARTESIAN_POINT('Ctrl Pts',(2.8414185613243,7.92041022602773,0.282539123257847));
#21962=CARTESIAN_POINT('Ctrl Pts',(2.56564497161068,8.09988309281573,0.285735047288138));
#21963=CARTESIAN_POINT('Ctrl Pts',(2.36305161962877,8.294962421875,0.289133913060426));
#21964=CARTESIAN_POINT('Ctrl Pts',(2.36305161962877,11.694962421875,0.3432986322892));
#21965=CARTESIAN_POINT('Ctrl Pts',(2.56564335337965,11.8900401927221,0.346161211451081));
#21966=CARTESIAN_POINT('Ctrl Pts',(2.84141117550506,12.0695095495884,0.348754767692783));
#21967=CARTESIAN_POINT('Ctrl Pts',(3.36597543488952,12.2867814488469,0.351879509430406));
#21968=CARTESIAN_POINT('Ctrl Pts',(3.7087541062761,12.354962421875,0.35285061152936));
#21969=CARTESIAN_POINT('Ctrl Pts',(4.,12.354962421875,0.35285061152936));
#21970=CARTESIAN_POINT('Ctrl Pts',(4.2912458937239,12.354962421875,0.35285061152936));
#21971=CARTESIAN_POINT('Ctrl Pts',(4.63402456511048,12.2867814488469,0.351879509430406));
#21972=CARTESIAN_POINT('Ctrl Pts',(5.15858882449494,12.0695095495884,0.348754767692784));
#21973=CARTESIAN_POINT('Ctrl Pts',(5.43435664662035,11.8900401927221,0.34616121145108));
#21974=CARTESIAN_POINT('Ctrl Pts',(5.63694838037123,11.694962421875,0.343298632289199));
#21975=CARTESIAN_POINT('Origin',(4.,0.,0.));
#21976=CARTESIAN_POINT('Origin',(0.,13.7,0.));
#21977=CARTESIAN_POINT('',(3.81639164714898E-16,-13.7,-1.67776611483187E-15));
#21978=CARTESIAN_POINT('Origin',(0.,0.,0.));
#21979=CARTESIAN_POINT('Origin',(0.15,0.,0.));
#21980=CARTESIAN_POINT('',(0.300000000000001,-14.,-1.71450551880629E-15));
#21981=CARTESIAN_POINT('Origin',(0.3,0.,0.));
#21982=CARTESIAN_POINT('',(0.15,-13.85,-1.69613581681908E-15));
#21983=CARTESIAN_POINT('Origin',(4.,0.,0.));
#21984=CARTESIAN_POINT('',(7.7,-14.,-1.71450551880629E-15));
#21985=CARTESIAN_POINT('Origin',(7.7,0.,0.));
#21986=CARTESIAN_POINT('',(4.,-14.,-1.71450551880629E-15));
#21987=CARTESIAN_POINT('Origin',(7.85,0.,0.));
#21988=CARTESIAN_POINT('',(8.,-13.7,-1.67776611483187E-15));
#21989=CARTESIAN_POINT('Origin',(8.,0.,0.));
#21990=CARTESIAN_POINT('',(7.85,-13.85,-1.69613581681908E-15));
#21991=CARTESIAN_POINT('Origin',(8.,12.6,0.));
#21992=CARTESIAN_POINT('',(8.,-12.6,-1.54305496692567E-15));
#21993=CARTESIAN_POINT('Origin',(8.,0.,0.));
#21994=CARTESIAN_POINT('Origin',(7.1,0.,0.));
#21995=CARTESIAN_POINT('',(7.1,-12.6,-1.54305496692567E-15));
#21996=CARTESIAN_POINT('Origin',(4.,0.,0.));
#21997=CARTESIAN_POINT('Origin',(8.,6.3,0.));
#21998=CARTESIAN_POINT('',(8.,-6.3,-7.71527483462833E-16));
#21999=CARTESIAN_POINT('Origin',(8.,0.,0.));
#22000=CARTESIAN_POINT('Origin',(7.85,0.,0.));
#22001=CARTESIAN_POINT('',(7.7,-6.,-7.34788079488412E-16));
#22002=CARTESIAN_POINT('',(7.85,-6.15,-7.53157781475622E-16));
#22003=CARTESIAN_POINT('Origin',(7.7,0.,0.));
#22004=CARTESIAN_POINT('Origin',(4.,0.,0.));
#22005=CARTESIAN_POINT('',(0.3,-6.,-7.34788079488412E-16));
#22006=CARTESIAN_POINT('',(4.,-6.,-7.34788079488412E-16));
#22007=CARTESIAN_POINT('Origin',(0.3,0.,0.));
#22008=CARTESIAN_POINT('Origin',(0.15,0.,0.));
#22009=CARTESIAN_POINT('',(-6.93889390390723E-17,-6.3,-7.71527483462833E-16));
#22010=CARTESIAN_POINT('',(0.15,-6.15,-7.53157781475622E-16));
#22011=CARTESIAN_POINT('Origin',(0.,0.,0.));
#22012=CARTESIAN_POINT('Origin',(0.,8.3,0.));
#22013=CARTESIAN_POINT('',(0.,0.,0.));
#22014=CARTESIAN_POINT('Origin',(0.,8.4,0.));
#22015=CARTESIAN_POINT('',(-3.12250225675825E-16,-8.4,-1.02870331128378E-15));
#22016=CARTESIAN_POINT('Origin',(0.,0.,0.));
#22017=CARTESIAN_POINT('',(-6.93889390390723E-17,-6.3,-7.71527483462833E-16));
#22018=CARTESIAN_POINT('Origin',(0.,0.,0.));
#22019=CARTESIAN_POINT('Origin',(0.2,0.,0.));
#22020=CARTESIAN_POINT('',(0.4,-8.7,-1.0654427152582E-15));
#22021=CARTESIAN_POINT('Origin',(0.4,0.,0.));
#22022=CARTESIAN_POINT('',(0.2,-8.55,-1.04707301327099E-15));
#22023=CARTESIAN_POINT('Origin',(0.4,11.5,0.));
#22024=CARTESIAN_POINT('',(0.4,-11.5,-1.40834381901946E-15));
#22025=CARTESIAN_POINT('Origin',(0.4,0.,0.));
#22026=CARTESIAN_POINT('Origin',(0.2,0.,0.));
#22027=CARTESIAN_POINT('',(-4.5102810375397E-16,-11.8,-1.44508322299388E-15));
#22028=CARTESIAN_POINT('',(0.2,-11.65,-1.42671352100667E-15));
#22029=CARTESIAN_POINT('Origin',(0.,0.,0.));
#22030=CARTESIAN_POINT('Origin',(0.,13.7,0.));
#22031=CARTESIAN_POINT('',(2.94902990916057E-16,-13.7,-1.67776611483187E-15));
#22032=CARTESIAN_POINT('Origin',(0.,0.,0.));
#22033=CARTESIAN_POINT('Origin',(0.15,0.,0.));
#22034=CARTESIAN_POINT('',(0.300000000000001,-14.,-1.71450551880629E-15));
#22035=CARTESIAN_POINT('Origin',(0.3,0.,0.));
#22036=CARTESIAN_POINT('',(0.15,-13.85,-1.69613581681908E-15));
#22037=CARTESIAN_POINT('Origin',(4.,0.,0.));
#22038=CARTESIAN_POINT('',(7.7,-14.,-1.71450551880629E-15));
#22039=CARTESIAN_POINT('Origin',(7.7,0.,0.));
#22040=CARTESIAN_POINT('',(4.,-14.,-1.71450551880629E-15));
#22041=CARTESIAN_POINT('Origin',(7.85,0.,0.));
#22042=CARTESIAN_POINT('',(8.,-13.7,-1.67776611483187E-15));
#22043=CARTESIAN_POINT('Origin',(8.,0.,0.));
#22044=CARTESIAN_POINT('',(7.85,-13.85,-1.69613581681908E-15));
#22045=CARTESIAN_POINT('Origin',(8.,11.8,0.));
#22046=CARTESIAN_POINT('',(8.,-11.8,-1.44508322299388E-15));
#22047=CARTESIAN_POINT('Origin',(8.,0.,0.));
#22048=CARTESIAN_POINT('Origin',(7.8,0.,0.));
#22049=CARTESIAN_POINT('',(7.6,-11.5,-1.40834381901946E-15));
#22050=CARTESIAN_POINT('',(7.8,-11.65,-1.42671352100667E-15));
#22051=CARTESIAN_POINT('Origin',(7.6,0.,0.));
#22052=CARTESIAN_POINT('Origin',(7.6,8.7,0.));
#22053=CARTESIAN_POINT('',(7.6,-8.7,-1.0654427152582E-15));
#22054=CARTESIAN_POINT('Origin',(7.6,0.,0.));
#22055=CARTESIAN_POINT('Origin',(7.8,0.,0.));
#22056=CARTESIAN_POINT('',(8.,-8.4,-1.02870331128378E-15));
#22057=CARTESIAN_POINT('Origin',(8.,0.,0.));
#22058=CARTESIAN_POINT('',(7.8,-8.55,-1.04707301327099E-15));
#22059=CARTESIAN_POINT('Origin',(8.,6.3,0.));
#22060=CARTESIAN_POINT('',(8.,-6.3,-7.71527483462833E-16));
#22061=CARTESIAN_POINT('Origin',(8.,0.,0.));
#22062=CARTESIAN_POINT('Origin',(7.85,0.,0.));
#22063=CARTESIAN_POINT('',(7.7,-6.,-7.34788079488412E-16));
#22064=CARTESIAN_POINT('',(7.85,-6.15,-7.53157781475622E-16));
#22065=CARTESIAN_POINT('Origin',(7.7,0.,0.));
#22066=CARTESIAN_POINT('Origin',(4.,0.,0.));
#22067=CARTESIAN_POINT('',(0.3,-6.,-7.34788079488412E-16));
#22068=CARTESIAN_POINT('',(4.,-6.,-7.34788079488412E-16));
#22069=CARTESIAN_POINT('Origin',(0.3,0.,0.));
#22070=CARTESIAN_POINT('Origin',(0.15,0.,0.));
#22071=CARTESIAN_POINT('',(0.15,-6.15,-7.53157781475622E-16));
#22072=CARTESIAN_POINT('',(0.,0.,0.));
#22073=CARTESIAN_POINT('Origin',(0.25,0.,0.));
#22074=CARTESIAN_POINT('',(0.5,-9.,-1.10218211923262E-15));
#22075=CARTESIAN_POINT('Origin',(0.5,0.,0.));
#22076=CARTESIAN_POINT('',(0.,-9.,-1.10218211923262E-15));
#22077=CARTESIAN_POINT('',(0.25,-9.,-1.10218211923262E-15));
#22078=CARTESIAN_POINT('Origin',(0.,0.,0.));
#22079=CARTESIAN_POINT('Origin',(0.5,6.,0.));
#22080=CARTESIAN_POINT('',(0.5,-6.,-7.34788079488412E-16));
#22081=CARTESIAN_POINT('Origin',(0.5,0.,0.));
#22082=CARTESIAN_POINT('Origin',(0.25,0.,0.));
#22083=CARTESIAN_POINT('',(0.,-6.,-7.34788079488412E-16));
#22084=CARTESIAN_POINT('',(0.25,-6.,-7.34788079488412E-16));
#22085=CARTESIAN_POINT('Origin',(0.,0.,0.));
#22086=CARTESIAN_POINT('Origin',(0.,9.,0.));
#22087=CARTESIAN_POINT('',(0.,0.,0.));
#22088=CARTESIAN_POINT('Origin',(2.025,0.,0.));
#22089=CARTESIAN_POINT('',(0.634469692124231,-1.95442077682041,0.00165102877781057));
#22090=CARTESIAN_POINT('',(0.53273030787577,-1.95523081632926,0.00202491348536037));
#22091=CARTESIAN_POINT('',(2.025,-1.954,-2.39295984553393E-16));
#22092=CARTESIAN_POINT('',(0.408600000000001,0.862482803259043,1.75460523117329));
#22093=CARTESIAN_POINT('Ctrl Pts',(0.634469692124231,-1.95442077682041,
0.00165102877781057));
#22094=CARTESIAN_POINT('Ctrl Pts',(0.626966520753468,-1.95553671624047,
0.133139557122026));
#22095=CARTESIAN_POINT('Ctrl Pts',(0.619463349382705,-1.94333788513784,
0.26441413153127));
#22096=CARTESIAN_POINT('Ctrl Pts',(0.611960178011943,-1.91704116468773,
0.392788375779545));
#22097=CARTESIAN_POINT('Ctrl Pts',(0.575840656321609,-1.7904513644889,1.01076923620262));
#22098=CARTESIAN_POINT('Ctrl Pts',(0.539721134631274,-1.337162156549,1.561538890573));
#22099=CARTESIAN_POINT('Ctrl Pts',(0.503601612940941,-0.75508611564872,
1.80514346557071));
#22100=CARTESIAN_POINT('Ctrl Pts',(0.471934408627294,-0.244760395632316,
2.01871982226583));
#22101=CARTESIAN_POINT('Ctrl Pts',(0.440267204313647,0.364558881626702,
1.99619002455956));
#22102=CARTESIAN_POINT('Ctrl Pts',(0.408600000000001,0.863439746847564,
1.75538915071904));
#22103=CARTESIAN_POINT('',(0.408600000000001,-0.861525859670526,1.75382131162754));
#22104=CARTESIAN_POINT('Origin',(0.408600000000001,0.,0.));
#22105=CARTESIAN_POINT('Ctrl Pts',(0.408600000000001,-0.861525859670528,
1.75382131162754));
#22106=CARTESIAN_POINT('Ctrl Pts',(0.444719521690335,-1.43012887970028,
1.47450767665535));
#22107=CARTESIAN_POINT('Ctrl Pts',(0.480839043380669,-1.84834511638748,
0.900224305747275));
#22108=CARTESIAN_POINT('Ctrl Pts',(0.516958565071003,-1.9370954607764,0.276569295008137));
#22109=CARTESIAN_POINT('Ctrl Pts',(0.522215812672592,-1.95001319925531,
0.18579542381635));
#22110=CARTESIAN_POINT('Ctrl Pts',(0.527473060274181,-1.95595113187234,
0.0939756038050989));
#22111=CARTESIAN_POINT('Ctrl Pts',(0.53273030787577,-1.95523081632926,0.00202491348536037));
#22112=CARTESIAN_POINT('Origin',(2.025,0.,0.));
#22113=CARTESIAN_POINT('',(1.33446969212423,-1.9523906058954,-0.00132468018748402));
#22114=CARTESIAN_POINT('',(1.23273030787577,-1.95165222738269,-0.000920442742864252));
#22115=CARTESIAN_POINT('',(2.025,-1.954,-2.39295984553393E-16));
#22116=CARTESIAN_POINT('Ctrl Pts',(1.33446969212423,-1.9523906058954,-0.00132468018748402));
#22117=CARTESIAN_POINT('Ctrl Pts',(1.31035031756214,-1.94957125408737,0.422486472286078));
#22118=CARTESIAN_POINT('Ctrl Pts',(1.28623094300005,-1.81322651205539,0.847951210739301));
#22119=CARTESIAN_POINT('Ctrl Pts',(1.26211156843795,-1.55843747807863,1.18346739203252));
#22120=CARTESIAN_POINT('Ctrl Pts',(1.22599204674762,-1.1768828894432,1.685913421737));
#22121=CARTESIAN_POINT('Ctrl Pts',(1.18987252505729,-0.529705083115927,
1.98664078026466));
#22122=CARTESIAN_POINT('Ctrl Pts',(1.15375300336695,0.100367612944418,1.95428499231951));
#22123=CARTESIAN_POINT('Ctrl Pts',(1.11763348167662,0.730440309004762,1.92192920437435));
#22124=CARTESIAN_POINT('Ctrl Pts',(1.08151395998628,1.34340789479817,1.55649026995639));
#22125=CARTESIAN_POINT('Ctrl Pts',(1.04539443829595,1.6714805104491,1.01759080735173));
#22126=CARTESIAN_POINT('Ctrl Pts',(1.00927491660562,1.99955312610003,0.478691344747064));
#22127=CARTESIAN_POINT('Ctrl Pts',(0.973155394915283,2.04273077160847,-0.233668646044295));
#22128=CARTESIAN_POINT('Ctrl Pts',(0.937035873224949,1.78215915473901,-0.808233567143524));
#22129=CARTESIAN_POINT('Ctrl Pts',(0.900916351534615,1.52158753786956,-1.38279848824275));
#22130=CARTESIAN_POINT('Ctrl Pts',(0.864796829844281,0.957266658622202,
-1.81956833964985));
#22131=CARTESIAN_POINT('Ctrl Pts',(0.828677308153947,0.33571329746904,-1.92782633644309));
#22132=CARTESIAN_POINT('Ctrl Pts',(0.792557786463613,-0.285840063684128,
-2.03608433323634));
#22133=CARTESIAN_POINT('Ctrl Pts',(0.756438264773278,-0.964625906743106,
-1.81583047541573));
#22134=CARTESIAN_POINT('Ctrl Pts',(0.720318743082944,-1.40407363204372,
-1.36310751326752));
#22135=CARTESIAN_POINT('Ctrl Pts',(0.691702392763373,-1.75223411329688,
-1.00442948331969));
#22136=CARTESIAN_POINT('Ctrl Pts',(0.663086042443802,-1.95016469471835,
-0.499833157597696));
#22137=CARTESIAN_POINT('Ctrl Pts',(0.634469692124231,-1.95442077682041,
0.00165102877781057));
#22138=CARTESIAN_POINT('Ctrl Pts',(0.53273030787577,-1.95523081632926,0.00202491348536037));
#22139=CARTESIAN_POINT('Ctrl Pts',(0.563592581964515,-1.95100225845912,
-0.537764653671288));
#22140=CARTESIAN_POINT('Ctrl Pts',(0.59445485605326,-1.71731794149376,-1.08206425789097));
#22141=CARTESIAN_POINT('Ctrl Pts',(0.625317130142005,-1.31923087498139,
-1.44574814791387));
#22142=CARTESIAN_POINT('Ctrl Pts',(0.661436651832339,-0.853331492706804,
-1.87138392952654));
#22143=CARTESIAN_POINT('Ctrl Pts',(0.697556173522673,-0.162248276066999,
-2.04962884218167));
#22144=CARTESIAN_POINT('Ctrl Pts',(0.733675695213007,0.451679724322199,
-1.9038608795556));
#22145=CARTESIAN_POINT('Ctrl Pts',(0.769795216903341,1.0656077247114,-1.75809291692952));
#22146=CARTESIAN_POINT('Ctrl Pts',(0.805914738593676,1.60238050884999,-1.28831207902223));
#22147=CARTESIAN_POINT('Ctrl Pts',(0.842034260284009,1.8277202876157,-0.699119771386502));
#22148=CARTESIAN_POINT('Ctrl Pts',(0.878153781974343,2.0530600663814,-0.109927463750781));
#22149=CARTESIAN_POINT('Ctrl Pts',(0.914273303664676,1.96696683977422,0.598676313613372));
#22150=CARTESIAN_POINT('Ctrl Pts',(0.95039282535501,1.60693687797777,1.11679866753813));
#22151=CARTESIAN_POINT('Ctrl Pts',(0.986512347045345,1.24690691618132,1.63492102146289));
#22152=CARTESIAN_POINT('Ctrl Pts',(1.02263186873568,0.612940219195604,1.96256195194826));
#22153=CARTESIAN_POINT('Ctrl Pts',(1.05875139042601,-0.0179439077178916,
1.95675679282911));
#22154=CARTESIAN_POINT('Ctrl Pts',(1.09487091211635,-0.648828034631387,
1.95095163370997));
#22155=CARTESIAN_POINT('Ctrl Pts',(1.13099043380668,-1.27662959147266,1.61170038498632));
#22156=CARTESIAN_POINT('Ctrl Pts',(1.16710995549701,-1.62711418555438,1.08712141076958));
#22157=CARTESIAN_POINT('Ctrl Pts',(1.18898340628993,-1.83936249792265,0.769444103802367));
#22158=CARTESIAN_POINT('Ctrl Pts',(1.21085685708285,-1.94990937996376,0.383800904758547));
#22159=CARTESIAN_POINT('Ctrl Pts',(1.23273030787577,-1.95165222738269,-0.000920442742864252));
#22160=CARTESIAN_POINT('Origin',(2.025,0.,0.));
#22161=CARTESIAN_POINT('',(2.03446969212423,-1.95576993562625,0.00117566504278285));
#22162=CARTESIAN_POINT('',(1.93273030787577,-1.95653837240827,0.000668140733460532));
#22163=CARTESIAN_POINT('',(2.025,-1.954,-2.39295984553393E-16));
#22164=CARTESIAN_POINT('Ctrl Pts',(2.03446969212423,-1.95576993562625,0.00117566504278285));
#22165=CARTESIAN_POINT('Ctrl Pts',(2.02985363606114,-1.95635392431848,0.0819247817601888));
#22166=CARTESIAN_POINT('Ctrl Pts',(2.02523757999806,-1.95176291393843,0.162607088786322));
#22167=CARTESIAN_POINT('Ctrl Pts',(2.02062152393497,-1.94176643790063,0.242614011988077));
#22168=CARTESIAN_POINT('Ctrl Pts',(1.98450200224464,-1.86354643187397,0.868648825791863));
#22169=CARTESIAN_POINT('Ctrl Pts',(1.9483824805543,-1.45436685550396,1.45333202356739));
#22170=CARTESIAN_POINT('Ctrl Pts',(1.91226295886397,-0.892984570149823,
1.74123449713021));
#22171=CARTESIAN_POINT('Ctrl Pts',(1.87614343717363,-0.331602284795679,
2.02913697069302));
#22172=CARTESIAN_POINT('Ctrl Pts',(1.8400239154833,0.381982709542597,2.02025872004313));
#22173=CARTESIAN_POINT('Ctrl Pts',(1.80390439379297,0.936028534854556,1.71847869934669));
#22174=CARTESIAN_POINT('Ctrl Pts',(1.76778487210263,1.49007436016651,1.41669867865025));
#22175=CARTESIAN_POINT('Ctrl Pts',(1.73166535041229,1.88458101645215,0.822016887907262));
#22176=CARTESIAN_POINT('Ctrl Pts',(1.69554582872196,1.94720150826564,0.194229666915167));
#22177=CARTESIAN_POINT('Ctrl Pts',(1.65942630703163,2.00982200007913,-0.433557554076929));
#22178=CARTESIAN_POINT('Ctrl Pts',(1.6233067853413,1.74055632742047,-1.09445020531813));
#22179=CARTESIAN_POINT('Ctrl Pts',(1.58718726365096,1.25703793962356,-1.49972501984526));
#22180=CARTESIAN_POINT('Ctrl Pts',(1.55106774196063,0.773519551826663,-1.90499983437239));
#22181=CARTESIAN_POINT('Ctrl Pts',(1.51494822027029,0.0757484488915239,
-2.05465681218543));
#22182=CARTESIAN_POINT('Ctrl Pts',(1.47882869857996,-0.531442461668977,
-1.88331767599797));
#22183=CARTESIAN_POINT('Ctrl Pts',(1.44270917688962,-1.13863337222948,-1.7119785398105));
#22184=CARTESIAN_POINT('Ctrl Pts',(1.40658965519929,-1.65524409041534,-1.21964328962253));
#22185=CARTESIAN_POINT('Ctrl Pts',(1.37047013350896,-1.85558376403649,-0.621393314087894));
#22186=CARTESIAN_POINT('Ctrl Pts',(1.35846998638071,-1.92214349258685,-0.422634100512704));
#22187=CARTESIAN_POINT('Ctrl Pts',(1.34646983925247,-1.95379332205687,-0.212184052646743));
#22188=CARTESIAN_POINT('Ctrl Pts',(1.33446969212423,-1.9523906058954,-0.00132468018748402));
#22189=CARTESIAN_POINT('Ctrl Pts',(1.23273030787577,-1.95165222738269,-0.000920442742864252));
#22190=CARTESIAN_POINT('Ctrl Pts',(1.24697637877319,-1.95278733533289,-0.251487563776593));
#22191=CARTESIAN_POINT('Ctrl Pts',(1.2612224496706,-1.90776937317109,-0.501663648953817));
#22192=CARTESIAN_POINT('Ctrl Pts',(1.27546852056802,-1.81463610591833,-0.732417095986825));
#22193=CARTESIAN_POINT('Ctrl Pts',(1.31158804225835,-1.57850580087837,-1.31746992881668));
#22194=CARTESIAN_POINT('Ctrl Pts',(1.34770756394868,-1.03307755947628,-1.77766889476657));
#22195=CARTESIAN_POINT('Ctrl Pts',(1.38382708563902,-0.416639625931859,
-1.91199265209425));
#22196=CARTESIAN_POINT('Ctrl Pts',(1.41994660732935,0.199798307612564,-2.04631640942193));
#22197=CARTESIAN_POINT('Ctrl Pts',(1.45606612901969,0.887245933299322,-1.85476495812738));
#22198=CARTESIAN_POINT('Ctrl Pts',(1.49218565071002,1.34538450854715,-1.42100803903579));
#22199=CARTESIAN_POINT('Ctrl Pts',(1.52830517240036,1.80352308379497,-0.987251119944189));
#22200=CARTESIAN_POINT('Ctrl Pts',(1.56442469409069,2.03235260860386,-0.311288733055544));
#22201=CARTESIAN_POINT('Ctrl Pts',(1.60054421578102,1.93190264788241,0.311566717611194));
#22202=CARTESIAN_POINT('Ctrl Pts',(1.63666373747136,1.83145268716095,0.934422168277935));
#22203=CARTESIAN_POINT('Ctrl Pts',(1.67278325916169,1.40172324090913,1.50417068272276));
#22204=CARTESIAN_POINT('Ctrl Pts',(1.70890278085203,0.830450180305799,1.77191139223846));
#22205=CARTESIAN_POINT('Ctrl Pts',(1.74502230254236,0.259177119702472,2.03965210175416));
#22206=CARTESIAN_POINT('Ctrl Pts',(1.78114182423269,-0.453639555252363,
2.00538500634072));
#22207=CARTESIAN_POINT('Ctrl Pts',(1.81726134592303,-0.996594329999513,
1.68407843139874));
#22208=CARTESIAN_POINT('Ctrl Pts',(1.85338086761336,-1.53954910474667,1.36277185645676));
#22209=CARTESIAN_POINT('Ctrl Pts',(1.8895003893037,-1.91264197928614,0.754425801986236));
#22210=CARTESIAN_POINT('Ctrl Pts',(1.92561991099403,-1.95288065385836,0.124807613218624));
#22211=CARTESIAN_POINT('Ctrl Pts',(1.92799004328794,-1.95552108146107,0.0834926031576606));
#22212=CARTESIAN_POINT('Ctrl Pts',(1.93036017558186,-1.95672828122377,0.0420859979926118));
#22213=CARTESIAN_POINT('Ctrl Pts',(1.93273030787577,-1.95653837240827,0.000668140733460532));
#22214=CARTESIAN_POINT('Origin',(2.025,0.,0.));
#22215=CARTESIAN_POINT('',(2.73446969212423,-1.95150456667077,-0.000783624415817835));
#22216=CARTESIAN_POINT('',(2.63273030787577,-1.95117066719132,-0.000238996725395994));
#22217=CARTESIAN_POINT('',(2.025,-1.954,-2.39295984553393E-16));
#22218=CARTESIAN_POINT('Ctrl Pts',(2.73446969212423,-1.95150456667077,-0.000783624415817835));
#22219=CARTESIAN_POINT('Ctrl Pts',(2.71323743286981,-1.9500751429531,0.372726459605641));
#22220=CARTESIAN_POINT('Ctrl Pts',(2.6920051736154,-1.84631774470697,0.746969407126199));
#22221=CARTESIAN_POINT('Ctrl Pts',(2.67077291436098,-1.64564170315827,1.05885167694053));
#22222=CARTESIAN_POINT('Ctrl Pts',(2.63465339267065,-1.30425916121605,1.58941407609013));
#22223=CARTESIAN_POINT('Ctrl Pts',(2.59853387098031,-0.682398562187567,
1.93950756724007));
#22224=CARTESIAN_POINT('Ctrl Pts',(2.56241434928998,-0.0517180701627423,
1.95618191441976));
#22225=CARTESIAN_POINT('Ctrl Pts',(2.52629482759964,0.578962421862082,1.97285626159946));
#22226=CARTESIAN_POINT('Ctrl Pts',(2.49017530590931,1.21846280688325,1.65611146480892));
#22227=CARTESIAN_POINT('Ctrl Pts',(2.45405578421898,1.58740000205626,1.14432599796594));
#22228=CARTESIAN_POINT('Ctrl Pts',(2.41793626252864,1.95633719722927,0.63254053112295));
#22229=CARTESIAN_POINT('Ctrl Pts',(2.38181674083831,2.05471120255412,-0.0742856057724776));
#22230=CARTESIAN_POINT('Ctrl Pts',(2.34569721914798,1.83954900887748,-0.667364969659822));
#22231=CARTESIAN_POINT('Ctrl Pts',(2.30957769745764,1.62438681520084,-1.26044433354716));
#22232=CARTESIAN_POINT('Ctrl Pts',(2.27345817576731,1.0956884225227,-1.73977692442642));
#22233=CARTESIAN_POINT('Ctrl Pts',(2.23733865407697,0.484423001993893,-1.8959572442284));
#22234=CARTESIAN_POINT('Ctrl Pts',(2.20121913238664,-0.126842418534916,
-2.05213756403038));
#22235=CARTESIAN_POINT('Ctrl Pts',(2.1650996106963,-0.820674866914401,-1.88516561275509));
#22236=CARTESIAN_POINT('Ctrl Pts',(2.12898008900597,-1.29396087326249,-1.46798642220142));
#22237=CARTESIAN_POINT('Ctrl Pts',(2.09747662337872,-1.70676117445901,-1.10412251495796));
#22238=CARTESIAN_POINT('Ctrl Pts',(2.06597315775148,-1.95178435411669,-0.549917516705958));
#22239=CARTESIAN_POINT('Ctrl Pts',(2.03446969212423,-1.95576993562625,0.00117566504278285));
#22240=CARTESIAN_POINT('Ctrl Pts',(1.93273030787577,-1.95653837240827,0.000668140733460532));
#22241=CARTESIAN_POINT('Ctrl Pts',(1.96647969727219,-1.95383417459587,-0.589099525904457));
#22242=CARTESIAN_POINT('Ctrl Pts',(2.00022908666861,-1.66784938341305,-1.18114869016093));
#22243=CARTESIAN_POINT('Ctrl Pts',(2.03397847606503,-1.20286828249105,-1.54351134325543));
#22244=CARTESIAN_POINT('Ctrl Pts',(2.07009799775536,-0.705232761946527,
-1.93132178789718));
#22245=CARTESIAN_POINT('Ctrl Pts',(2.1062175194457,-0.002577246252485,-2.05605235411599));
#22246=CARTESIAN_POINT('Ctrl Pts',(2.14233704113603,0.598131172672099,-1.86321201845565));
#22247=CARTESIAN_POINT('Ctrl Pts',(2.17845656282637,1.19883959159669,-1.67037168279531));
#22248=CARTESIAN_POINT('Ctrl Pts',(2.2145760845167,1.69760091375181,-1.15996044525583));
#22249=CARTESIAN_POINT('Ctrl Pts',(2.25069560620703,1.87652291444005,-0.554960470090062));
#22250=CARTESIAN_POINT('Ctrl Pts',(2.28681512789737,2.05544491512828,0.0500395050757017));
#22251=CARTESIAN_POINT('Ctrl Pts',(2.3229346495877,1.91452759434962,0.749628217867738));
#22252=CARTESIAN_POINT('Ctrl Pts',(2.35905417127804,1.51533268176147,1.23817876420054));
#22253=CARTESIAN_POINT('Ctrl Pts',(2.39517369296837,1.11613776917333,1.72672931053334));
#22254=CARTESIAN_POINT('Ctrl Pts',(2.43129321465871,0.458665264775706,2.0042416904069));
#22255=CARTESIAN_POINT('Ctrl Pts',(2.46741273634904,-0.169855919296459,
1.94947926082059));
#22256=CARTESIAN_POINT('Ctrl Pts',(2.50353225803937,-0.798377103368625,
1.89471683123428));
#22257=CARTESIAN_POINT('Ctrl Pts',(2.53965177972971,-1.39794696711534,1.50767959218809));
#22258=CARTESIAN_POINT('Ctrl Pts',(2.57577130142004,-1.7066347542496,0.957452505089308));
#22259=CARTESIAN_POINT('Ctrl Pts',(2.59475763690528,-1.86889742032186,0.668223977693796));
#22260=CARTESIAN_POINT('Ctrl Pts',(2.61374397239053,-1.95078614203936,0.333904285110699));
#22261=CARTESIAN_POINT('Ctrl Pts',(2.63273030787577,-1.95117066719132,-0.000238996725395994));
#22262=CARTESIAN_POINT('Origin',(2.025,0.,0.));
#22263=CARTESIAN_POINT('',(3.43446969212423,-1.95694215816793,0.000613609334558611));
#22264=CARTESIAN_POINT('',(3.33273030787577,-1.95689202958038,-0.000120183693368507));
#22265=CARTESIAN_POINT('',(2.025,-1.954,-2.39295984553393E-16));
#22266=CARTESIAN_POINT('Ctrl Pts',(3.43446969212423,-1.95694215816793,0.000613609334558611));
#22267=CARTESIAN_POINT('Ctrl Pts',(3.43274075136882,-1.95706861247031,0.0308306145688404));
#22268=CARTESIAN_POINT('Ctrl Pts',(3.43101181061341,-1.95644434477529,0.0610420651850611));
#22269=CARTESIAN_POINT('Ctrl Pts',(3.42928286985799,-1.95505445535266,0.0912168450879343));
#22270=CARTESIAN_POINT('Ctrl Pts',(3.39316334816766,-1.92601809827063,0.721602018085349));
#22271=CARTESIAN_POINT('Ctrl Pts',(3.35704382647733,-1.56283440190639,1.33598265404732));
#22272=CARTESIAN_POINT('Ctrl Pts',(3.32092430478699,-1.02535127629691,1.66653914851539));
#22273=CARTESIAN_POINT('Ctrl Pts',(3.28480478309666,-0.48786815068743,1.99709564298347));
#22274=CARTESIAN_POINT('Ctrl Pts',(3.24868526140633,0.223914404167301,2.04382799595763));
#22275=CARTESIAN_POINT('Ctrl Pts',(3.21256573971599,0.799644251583046,1.78602872489919));
#22276=CARTESIAN_POINT('Ctrl Pts',(3.17644621802565,1.3753740989988,1.52822945384073));
#22277=CARTESIAN_POINT('Ctrl Pts',(3.14032669633532,1.81505123897556,0.965898558749655));
#22278=CARTESIAN_POINT('Ctrl Pts',(3.10420717464499,1.92628208012454,0.344850989150182));
#22279=CARTESIAN_POINT('Ctrl Pts',(3.06808765295465,2.03751292127353,-0.276196580449285));
#22280=CARTESIAN_POINT('Ctrl Pts',(3.03196813126432,1.82029746359473,-0.955960824557148));
#22281=CARTESIAN_POINT('Ctrl Pts',(2.99584860957399,1.36969361078797,-1.39755401117372));
#22282=CARTESIAN_POINT('Ctrl Pts',(2.95972908788365,0.919089757981196,-1.83914719779029));
#22283=CARTESIAN_POINT('Ctrl Pts',(2.92360956619332,0.235097510046449,-2.04256932691557));
#22284=CARTESIAN_POINT('Ctrl Pts',(2.88749004450298,-0.383555026741606,
-1.91891070488933));
#22285=CARTESIAN_POINT('Ctrl Pts',(2.85137052281265,-1.00220756352966,-1.79525208286309));
#22286=CARTESIAN_POINT('Ctrl Pts',(2.81525100112232,-1.55552038917102,-1.34451270968533));
#22287=CARTESIAN_POINT('Ctrl Pts',(2.77913147943199,-1.80172455956373,-0.763627369521821));
#22288=CARTESIAN_POINT('Ctrl Pts',(2.76424421699607,-1.90320170892571,-0.524205801918239));
#22289=CARTESIAN_POINT('Ctrl Pts',(2.74935695456015,-1.9525068248743,-0.262674861549822));
#22290=CARTESIAN_POINT('Ctrl Pts',(2.73446969212423,-1.95150456667077,-0.000783624415817835));
#22291=CARTESIAN_POINT('Ctrl Pts',(2.63273030787577,-1.95117066719132,-0.000238996725395994));
#22292=CARTESIAN_POINT('Ctrl Pts',(2.64986349408086,-1.95151766100874,-0.301768434637608));
#22293=CARTESIAN_POINT('Ctrl Pts',(2.66699668028595,-1.88549433057532,-0.603154218124976));
#22294=CARTESIAN_POINT('Ctrl Pts',(2.68412986649104,-1.75227012486661,-0.871132062271862));
#22295=CARTESIAN_POINT('Ctrl Pts',(2.72024938818138,-1.47141199782754,-1.43607260738287));
#22296=CARTESIAN_POINT('Ctrl Pts',(2.75636890987171,-0.89189003322759,-1.85253676245349));
#22297=CARTESIAN_POINT('Ctrl Pts',(2.79248843156204,-0.266884103330787,
-1.93858097541276));
#22298=CARTESIAN_POINT('Ctrl Pts',(2.82860795325238,0.358121826566009,-2.02462518837203));
#22299=CARTESIAN_POINT('Ctrl Pts',(2.86472747494271,1.02861172175966,-1.78024945921995));
#22300=CARTESIAN_POINT('Ctrl Pts',(2.90084699663305,1.45168171419148,-1.31222127716369));
#22301=CARTESIAN_POINT('Ctrl Pts',(2.93696651832338,1.87475170662331,-0.844193095107442));
#22302=CARTESIAN_POINT('Ctrl Pts',(2.97308604001372,2.0504017962933,-0.152512460147026));
#22303=CARTESIAN_POINT('Ctrl Pts',(3.00920556170405,1.90187502389171,0.460662992754071));
#22304=CARTESIAN_POINT('Ctrl Pts',(3.04532508339438,1.75334825149011,1.07383844565517));
#22305=CARTESIAN_POINT('Ctrl Pts',(3.08144460508472,1.28064461701691,1.60850871649694));
#22306=CARTESIAN_POINT('Ctrl Pts',(3.11756412677505,0.690313345419868,1.83106554216969));
#22307=CARTESIAN_POINT('Ctrl Pts',(3.15368364846538,0.099982073822824,2.05362236784244));
#22308=CARTESIAN_POINT('Ctrl Pts',(3.18980317015572,-0.607976834898069,
1.96406574834616));
#22309=CARTESIAN_POINT('Ctrl Pts',(3.22592269184605,-1.12435700524545,1.60157436757165));
#22310=CARTESIAN_POINT('Ctrl Pts',(3.26152523052262,-1.63334616474276,1.24427136908255));
#22311=CARTESIAN_POINT('Ctrl Pts',(3.2971277691992,-1.95620151659337,0.621790789891298));
#22312=CARTESIAN_POINT('Ctrl Pts',(3.33273030787577,-1.95689202958038,-0.000120183693368507));
#22313=CARTESIAN_POINT('Origin',(-0.885456225603702,0.,0.));
#22314=CARTESIAN_POINT('',(2.9645437743963,-1.55351348692753,-0.000623811555172185));
#22315=CARTESIAN_POINT('',(3.1026562256037,-1.5578012360145,-9.56321627601668E-5));
#22316=CARTESIAN_POINT('',(-0.885456225603702,-1.5555,-7.61108830709034E-15));
#22317=CARTESIAN_POINT('',(3.646,-1.53400205074397,0.257716818064529));
#22318=CARTESIAN_POINT('Ctrl Pts',(2.9645437743963,-1.55351348692753,-0.000623811555172191));
#22319=CARTESIAN_POINT('Ctrl Pts',(2.97943103683221,-1.554311343957,-0.209104783593014));
#22320=CARTESIAN_POINT('Ctrl Pts',(3.03043782095846,-1.41983356141065,-0.922420232737971));
#22321=CARTESIAN_POINT('Ctrl Pts',(3.11756412677505,-0.357346860176684,
-1.78794253319936));
#22322=CARTESIAN_POINT('Ctrl Pts',(3.22592269184605,1.2761484443205,-1.30213426013737));
#22323=CARTESIAN_POINT('Ctrl Pts',(3.33428125691706,1.79489764250785,0.32126381822974));
#22324=CARTESIAN_POINT('Ctrl Pts',(3.44263982198805,0.744870327409823,1.66421014471004));
#22325=CARTESIAN_POINT('Ctrl Pts',(3.54654606968238,-0.88514792232698,1.55719067973231));
#22326=CARTESIAN_POINT('Ctrl Pts',(3.61433279568635,-1.45984003145562,0.691579922874265));
#22327=CARTESIAN_POINT('Ctrl Pts',(3.646,-1.53590465648925,0.257207812787695));
#22328=CARTESIAN_POINT('',(3.646,-0.254962570226321,1.53446223081039));
#22329=CARTESIAN_POINT('Origin',(3.646,0.,0.));
#22330=CARTESIAN_POINT('Ctrl Pts',(3.1026562256037,-1.55780222723249,-9.5673354675919E-5));
#22331=CARTESIAN_POINT('Ctrl Pts',(3.10317320861747,-1.55781020924886,-0.00728468162261492));
#22332=CARTESIAN_POINT('Ctrl Pts',(3.13980971332156,-1.55454362905802,-0.516733977523194));
#22333=CARTESIAN_POINT('Ctrl Pts',(3.21256573971599,-1.00543213394195,-1.52103014244754));
#22334=CARTESIAN_POINT('Ctrl Pts',(3.320924304787,0.68997158388018,-1.68716896408801));
#22335=CARTESIAN_POINT('Ctrl Pts',(3.429282869858,1.78424156303041,-0.380380645529688));
#22336=CARTESIAN_POINT('Ctrl Pts',(3.53764143492899,1.31614849123568,1.26120506567147));
#22337=CARTESIAN_POINT('Ctrl Pts',(3.60988047830967,0.242522465892156,1.61712315325676));
#22338=CARTESIAN_POINT('Ctrl Pts',(3.646,-0.254962570226321,1.53446223081039));
#22339=CARTESIAN_POINT('Origin',(-0.885456225603702,0.,0.));
#22340=CARTESIAN_POINT('',(2.2645437743963,-1.55690897383144,0.000935899167884407));
#22341=CARTESIAN_POINT('',(2.4026562256037,-1.5532476831198,-0.000190255581553472));
#22342=CARTESIAN_POINT('',(-0.885456225603702,-1.5555,-7.61108830709034E-15));
#22343=CARTESIAN_POINT('Ctrl Pts',(2.2645437743963,-1.55690897383144,0.000935899167884323));
#22344=CARTESIAN_POINT('Ctrl Pts',(2.29604724002354,-1.55373621434417,-0.437766989373654));
#22345=CARTESIAN_POINT('Ctrl Pts',(2.36367022734113,-1.13505001352398,-1.38477120961871));
#22346=CARTESIAN_POINT('Ctrl Pts',(2.46741273634904,0.451357723348635,-1.76654291251687));
#22347=CARTESIAN_POINT('Ctrl Pts',(2.57577130142004,1.71398364424552,-0.621811318178061));
#22348=CARTESIAN_POINT('Ctrl Pts',(2.68412986649104,1.47904899949198,1.06621537978638));
#22349=CARTESIAN_POINT('Ctrl Pts',(2.79248843156204,-0.0481918125352924,
1.82265836557096));
#22350=CARTESIAN_POINT('Ctrl Pts',(2.88595973419713,-1.32926753649534,1.10144162772121));
#22351=CARTESIAN_POINT('Ctrl Pts',(2.94331151514188,-1.55237558078994,0.296712388903057));
#22352=CARTESIAN_POINT('Ctrl Pts',(2.9645437743963,-1.55351348692753,-0.000623811555172191));
#22353=CARTESIAN_POINT('Ctrl Pts',(2.4026562256037,-1.5532476831198,-0.000190255581553507));
#22354=CARTESIAN_POINT('Ctrl Pts',(2.4197894118088,-1.5535239107979,-0.240225588576664));
#22355=CARTESIAN_POINT('Ctrl Pts',(2.47304211970422,-1.39016363968781,-0.985938702047525));
#22356=CARTESIAN_POINT('Ctrl Pts',(2.56241434928998,-0.248663526484289,
-1.80625943050602));
#22357=CARTESIAN_POINT('Ctrl Pts',(2.67077291436098,1.35258575494928,-1.22264666689896));
#22358=CARTESIAN_POINT('Ctrl Pts',(2.77913147943198,1.77206945169698,0.429209875088153));
#22359=CARTESIAN_POINT('Ctrl Pts',(2.88749004450298,0.643168985847878,1.70609770460869));
#22360=CARTESIAN_POINT('Ctrl Pts',(2.99533162656023,-1.03949642371216,1.49324096396001));
#22361=CARTESIAN_POINT('Ctrl Pts',(3.06705368692713,-1.55725253790225,0.494982381615103));
#22362=CARTESIAN_POINT('Ctrl Pts',(3.1026562256037,-1.55780222723249,-9.5673354675919E-5));
#22363=CARTESIAN_POINT('Origin',(-0.885456225603702,0.,0.));
#22364=CARTESIAN_POINT('',(1.5645437743963,-1.55421882675041,-0.00105452406940307));
#22365=CARTESIAN_POINT('',(1.7026562256037,-1.55752069512848,0.000531879688266731));
#22366=CARTESIAN_POINT('',(-0.885456225603702,-1.5555,-7.61108830709034E-15));
#22367=CARTESIAN_POINT('Ctrl Pts',(1.5645437743963,-1.55421882675041,-0.00105452406940303));
#22368=CARTESIAN_POINT('Ctrl Pts',(1.57654392152454,-1.55533547208775,-0.168911102298873));
#22369=CARTESIAN_POINT('Ctrl Pts',(1.62466359034311,-1.45430488205528,-0.840696475689404));
#22370=CARTESIAN_POINT('Ctrl Pts',(1.70890278085203,-0.495166959245057,
-1.75476463681813));
#22371=CARTESIAN_POINT('Ctrl Pts',(1.81726134592303,1.17123470495496,-1.39735712045959));
#22372=CARTESIAN_POINT('Ctrl Pts',(1.92561991099403,1.81428908646041,0.180972233182718));
#22373=CARTESIAN_POINT('Ctrl Pts',(2.03397847606503,0.872136931108851,1.60117826005178));
#22374=CARTESIAN_POINT('Ctrl Pts',(2.14233704113603,-0.832031122156023,
1.62238110378654));
#22375=CARTESIAN_POINT('Ctrl Pts',(2.21919214057979,-1.52512187202985,0.632012719372306));
#22376=CARTESIAN_POINT('Ctrl Pts',(2.25992771833321,-1.55737386349918,0.0652169897789001));
#22377=CARTESIAN_POINT('Ctrl Pts',(2.2645437743963,-1.55690897383144,0.000935899167884323));
#22378=CARTESIAN_POINT('Ctrl Pts',(1.7026562256037,-1.55752069512848,0.000531879688266792));
#22379=CARTESIAN_POINT('Ctrl Pts',(1.73640561500012,-1.55536799313402,-0.468958194751484));
#22380=CARTESIAN_POINT('Ctrl Pts',(1.80627452608688,-1.08405821641942,-1.44466937944663));
#22381=CARTESIAN_POINT('Ctrl Pts',(1.91226295886397,0.557303862904986,-1.73603266764626));
#22382=CARTESIAN_POINT('Ctrl Pts',(2.02062152393497,1.74843472771405,-0.517079730093531));
#22383=CARTESIAN_POINT('Ctrl Pts',(2.12898008900597,1.41189906885343,1.15366271015419));
#22384=CARTESIAN_POINT('Ctrl Pts',(2.23733865407697,-0.158262365011203,
1.81641169719614));
#22385=CARTESIAN_POINT('Ctrl Pts',(2.32856403294288,-1.36373938799973,1.03824633745719));
#22386=CARTESIAN_POINT('Ctrl Pts',(2.38366989011846,-1.55294157827136,0.265807633310998));
#22387=CARTESIAN_POINT('Ctrl Pts',(2.4026562256037,-1.5532476831198,-0.000190255581553507));
#22388=CARTESIAN_POINT('Origin',(-0.885456225603702,0.,0.));
#22389=CARTESIAN_POINT('',(0.864543774396297,-1.55583496332863,0.00131431692112688));
#22390=CARTESIAN_POINT('',(1.0026562256037,-1.55363103362015,-0.000732727065787808));
#22391=CARTESIAN_POINT('',(-0.885456225603702,-1.5555,-7.61108830709034E-15));
#22392=CARTESIAN_POINT('Ctrl Pts',(0.864543774396297,-1.55583496332863,
0.00131431692112695));
#22393=CARTESIAN_POINT('Ctrl Pts',(0.893160124715868,-1.55244686931136,
-0.39789686624525));
#22394=CARTESIAN_POINT('Ctrl Pts',(0.957895996725773,-1.19600466962952,
-1.30659638604676));
#22395=CARTESIAN_POINT('Ctrl Pts',(1.05875139042601,0.312808167767432,-1.79617914851027));
#22396=CARTESIAN_POINT('Ctrl Pts',(1.16710995549701,1.66050693082158,-0.753094956293683));
#22397=CARTESIAN_POINT('Ctrl Pts',(1.27546852056802,1.55739102357227,0.948147570332657));
#22398=CARTESIAN_POINT('Ctrl Pts',(1.38382708563902,0.093515261491943,1.82088082901303));
#22399=CARTESIAN_POINT('Ctrl Pts',(1.48018550358178,-1.28089611724802,1.18222619744519));
#22400=CARTESIAN_POINT('Ctrl Pts',(1.5404243998342,-1.55197445533925,0.336324313019962));
#22401=CARTESIAN_POINT('Ctrl Pts',(1.5645437743963,-1.55421882675041,-0.00105452406940303));
#22402=CARTESIAN_POINT('Ctrl Pts',(1.0026562256037,-1.55363103362015,-0.000732727065787947));
#22403=CARTESIAN_POINT('Ctrl Pts',(1.01690229650112,-1.55453464693465,-0.200199030427076));
#22404=CARTESIAN_POINT('Ctrl Pts',(1.06726788908887,-1.42783653745201,-0.904292141434522));
#22405=CARTESIAN_POINT('Ctrl Pts',(1.15375300336695,-0.388197806685981,
-1.78147566906063));
#22406=CARTESIAN_POINT('Ctrl Pts',(1.26211156843795,1.2535495552727,-1.3240166887812));
#22407=CARTESIAN_POINT('Ctrl Pts',(1.37047013350896,1.8000352141881,0.290301877450055));
#22408=CARTESIAN_POINT('Ctrl Pts',(1.47882869857996,0.773764763351813,1.65096279999703));
#22409=CARTESIAN_POINT('Ctrl Pts',(1.58718726365096,-0.928568406390638,
1.56912687330982));
#22410=CARTESIAN_POINT('Ctrl Pts',(1.66179643932554,-1.54206571520519,0.568789711399914));
#22411=CARTESIAN_POINT('Ctrl Pts',(1.70028609330979,-1.55767187381964,0.0335029528543981));
#22412=CARTESIAN_POINT('Ctrl Pts',(1.7026562256037,-1.55752069512848,0.000531879688266792));
#22413=CARTESIAN_POINT('Origin',(3.646,2.59090492670967E-16,0.));
#22414=CARTESIAN_POINT('',(3.646,0.629287956476874,-1.84989531266857));
#22415=CARTESIAN_POINT('Ctrl Pts',(3.646,-1.53590465648925,0.257207812787684));
#22416=CARTESIAN_POINT('Ctrl Pts',(3.646,-1.55437165720027,0.196895341718919));
#22417=CARTESIAN_POINT('Ctrl Pts',(3.646,-1.56896355683948,0.135616641599751));
#22418=CARTESIAN_POINT('Ctrl Pts',(3.646,-1.5794868132962,0.0736940107076772));
#22419=CARTESIAN_POINT('Ctrl Pts',(3.646,-1.58951842709423,0.014664382282102));
#22420=CARTESIAN_POINT('Ctrl Pts',(3.646,-1.5958536213326,-0.0449514371865003));
#22421=CARTESIAN_POINT('Ctrl Pts',(3.646,-1.59865979572508,-0.104879712275592));
#22422=CARTESIAN_POINT('Ctrl Pts',(3.646,-1.59931069948911,-0.118780323702925));
#22423=CARTESIAN_POINT('Ctrl Pts',(3.646,-1.59977152479897,-0.132697823616271));
#22424=CARTESIAN_POINT('Ctrl Pts',(3.646,-1.60004398707201,-0.146628916982726));
#22425=CARTESIAN_POINT('Ctrl Pts',(3.646,-1.60029819926649,-0.159626877312327));
#22426=CARTESIAN_POINT('Ctrl Pts',(3.646,-1.60038827226624,-0.172631782210399));
#22427=CARTESIAN_POINT('Ctrl Pts',(3.646,-1.60031610868448,-0.185632728843391));
#22428=CARTESIAN_POINT('Ctrl Pts',(3.646,-1.59997115748781,-0.247778924875277));
#22429=CARTESIAN_POINT('Ctrl Pts',(3.646,-1.59592448582643,-0.309888778101361));
#22430=CARTESIAN_POINT('Ctrl Pts',(3.646,-1.58837167340201,-0.371662510966953));
#22431=CARTESIAN_POINT('Ctrl Pts',(3.646,-1.58235446873971,-0.420876654324364));
#22432=CARTESIAN_POINT('Ctrl Pts',(3.646,-1.57411085537686,-0.469878150447174));
#22433=CARTESIAN_POINT('Ctrl Pts',(3.646,-1.56371690971211,-0.518521573067589));
#22434=CARTESIAN_POINT('Ctrl Pts',(3.646,-1.55949291302958,-0.538289778752235));
#22435=CARTESIAN_POINT('Ctrl Pts',(3.646,-1.55491355506823,-0.557998881141082));
#22436=CARTESIAN_POINT('Ctrl Pts',(3.646,-1.54998301914068,-0.577639185380113));
#22437=CARTESIAN_POINT('Ctrl Pts',(3.646,-1.54698757787163,-0.589571230642318));
#22438=CARTESIAN_POINT('Ctrl Pts',(3.646,-1.54386473422877,-0.601468946211907));
#22439=CARTESIAN_POINT('Ctrl Pts',(3.646,-1.54061666379623,-0.613327738526289));
#22440=CARTESIAN_POINT('Ctrl Pts',(3.646,-1.52355820100381,-0.675608643962078));
#22441=CARTESIAN_POINT('Ctrl Pts',(3.646,-1.50304441626246,-0.736836650927299));
#22442=CARTESIAN_POINT('Ctrl Pts',(3.646,-1.47927170237122,-0.796705417992335));
#22443=CARTESIAN_POINT('Ctrl Pts',(3.646,-1.45499081172395,-0.857853968088201));
#22444=CARTESIAN_POINT('Ctrl Pts',(3.646,-1.42731013062283,-0.917585613768136));
#22445=CARTESIAN_POINT('Ctrl Pts',(3.646,-1.39638521586208,-0.975578488374583));
#22446=CARTESIAN_POINT('Ctrl Pts',(3.646,-1.3746359269342,-1.01636449523448));
#22447=CARTESIAN_POINT('Ctrl Pts',(3.646,-1.35128083281079,-1.05629059526188));
#22448=CARTESIAN_POINT('Ctrl Pts',(3.646,-1.32635893912807,-1.09524162657284));
#22449=CARTESIAN_POINT('Ctrl Pts',(3.646,-1.31177207824354,-1.11803978478166));
#22450=CARTESIAN_POINT('Ctrl Pts',(3.646,-1.29664823418257,-1.14050383295085));
#22451=CARTESIAN_POINT('Ctrl Pts',(3.646,-1.28099334691039,-1.16260978006393));
#22452=CARTESIAN_POINT('Ctrl Pts',(3.646,-1.27439565977673,-1.17192623953817));
#22453=CARTESIAN_POINT('Ctrl Pts',(3.646,-1.26770344996135,-1.18117916964538));
#22454=CARTESIAN_POINT('Ctrl Pts',(3.646,-1.26092631253354,-1.1903547340509));
#22455=CARTESIAN_POINT('Ctrl Pts',(3.646,-1.22063806006406,-1.24490098742961));
#22456=CARTESIAN_POINT('Ctrl Pts',(3.646,-1.17727779039597,-1.2968210133787));
#22457=CARTESIAN_POINT('Ctrl Pts',(3.646,-1.13102406755431,-1.34578478738438));
#22458=CARTESIAN_POINT('Ctrl Pts',(3.646,-1.10889356311025,-1.36921193987413));
#22459=CARTESIAN_POINT('Ctrl Pts',(3.646,-1.08609991322821,-1.39196224634769));
#22460=CARTESIAN_POINT('Ctrl Pts',(3.646,-1.06265860358067,-1.41399845269635));
#22461=CARTESIAN_POINT('Ctrl Pts',(3.646,-1.01519019024582,-1.45862154615905));
#22462=CARTESIAN_POINT('Ctrl Pts',(3.646,-0.965068683520578,-1.50031866495972));
#22463=CARTESIAN_POINT('Ctrl Pts',(3.646,-0.912608878859399,-1.53907430433262));
#22464=CARTESIAN_POINT('Ctrl Pts',(3.646,-0.885622701907269,-1.55901083571632));
#22465=CARTESIAN_POINT('Ctrl Pts',(3.646,-0.858017059499759,-1.57816846922923));
#22466=CARTESIAN_POINT('Ctrl Pts',(3.646,-0.829830930562831,-1.59654158274954));
#22467=CARTESIAN_POINT('Ctrl Pts',(3.646,-0.814618170658192,-1.6064580123987));
#22468=CARTESIAN_POINT('Ctrl Pts',(3.646,-0.799236272325966,-1.61614586579418));
#22469=CARTESIAN_POINT('Ctrl Pts',(3.646,-0.783691102223765,-1.62560394324042));
#22470=CARTESIAN_POINT('Ctrl Pts',(3.646,-0.774136405388099,-1.63141726416602));
#22471=CARTESIAN_POINT('Ctrl Pts',(3.646,-0.764521109964347,-1.63714302305682));
#22472=CARTESIAN_POINT('Ctrl Pts',(3.646,-0.754857428305642,-1.64277491414178));
#22473=CARTESIAN_POINT('Ctrl Pts',(3.646,-0.696336086560278,-1.67688053087207));
#22474=CARTESIAN_POINT('Ctrl Pts',(3.646,-0.635940296883035,-1.70761001018091));
#22475=CARTESIAN_POINT('Ctrl Pts',(3.646,-0.574032023975561,-1.73496968591445));
#22476=CARTESIAN_POINT('Ctrl Pts',(3.646,-0.510809778563976,-1.76291005724725));
#22477=CARTESIAN_POINT('Ctrl Pts',(3.646,-0.44600942822765,-1.78733655318714));
#22478=CARTESIAN_POINT('Ctrl Pts',(3.646,-0.379975375970469,-1.80821892080948));
#22479=CARTESIAN_POINT('Ctrl Pts',(3.646,-0.313405396837469,-1.82927076799057));
#22480=CARTESIAN_POINT('Ctrl Pts',(3.646,-0.245580690800976,-1.84672118374022));
#22481=CARTESIAN_POINT('Ctrl Pts',(3.646,-0.176825498658314,-1.8604948666779));
#22482=CARTESIAN_POINT('Ctrl Pts',(3.646,-0.159462280356867,-1.86397322891076));
#22483=CARTESIAN_POINT('Ctrl Pts',(3.646,-0.14203961847147,-1.86721686959177));
#22484=CARTESIAN_POINT('Ctrl Pts',(3.646,-0.124562559998911,-1.87022407918187));
#22485=CARTESIAN_POINT('Ctrl Pts',(3.646,-0.111792875781347,-1.87242130916207));
#22486=CARTESIAN_POINT('Ctrl Pts',(3.646,-0.0989925581628777,-1.87449245974032));
#22487=CARTESIAN_POINT('Ctrl Pts',(3.646,-0.0861825093113372,-1.87643420987567));
#22488=CARTESIAN_POINT('Ctrl Pts',(3.646,-0.0148835153063319,-1.88724172769734));
#22489=CARTESIAN_POINT('Ctrl Pts',(3.646,0.0568426981623723,-1.89406743257586));
#22490=CARTESIAN_POINT('Ctrl Pts',(3.646,0.128627456019564,-1.89688915407946));
#22491=CARTESIAN_POINT('Ctrl Pts',(3.646,0.200626979511061,-1.89971931760928));
#22492=CARTESIAN_POINT('Ctrl Pts',(3.646,0.272686413280953,-1.89852190431662));
#22493=CARTESIAN_POINT('Ctrl Pts',(3.646,0.344457463266169,-1.89322793788438));
#22494=CARTESIAN_POINT('Ctrl Pts',(3.646,0.414769043130747,-1.88804162468877));
#22495=CARTESIAN_POINT('Ctrl Pts',(3.646,0.484804859069096,-1.87892387244832));
#22496=CARTESIAN_POINT('Ctrl Pts',(3.646,0.554245063947006,-1.86576101897151));
#22497=CARTESIAN_POINT('Ctrl Pts',(3.646,0.579342242418372,-1.86100368158346));
#22498=CARTESIAN_POINT('Ctrl Pts',(3.646,0.60436161907656,-1.85571746700255));
#22499=CARTESIAN_POINT('Ctrl Pts',(3.646,0.629287956476874,-1.84989531266857));
#22500=CARTESIAN_POINT('',(3.646,-1.954,-2.39295984553393E-16));
#22501=CARTESIAN_POINT('Origin',(3.646,0.,0.));
#22502=CARTESIAN_POINT('',(3.646,1.85122479320614,-0.632364557278426));
#22503=CARTESIAN_POINT('Origin',(3.646,0.,0.));
#22504=CARTESIAN_POINT('Ctrl Pts',(3.646,1.85122479320614,-0.632364557278413));
#22505=CARTESIAN_POINT('Ctrl Pts',(3.646,1.86777728496137,-0.56405200123613));
#22506=CARTESIAN_POINT('Ctrl Pts',(3.646,1.88043336182538,-0.494993211783664));
#22507=CARTESIAN_POINT('Ctrl Pts',(3.646,1.88896124154753,-0.425422790109387));
#22508=CARTESIAN_POINT('Ctrl Pts',(3.646,1.88988050194317,-0.41792346607611));
#22509=CARTESIAN_POINT('Ctrl Pts',(3.646,1.89075174381644,-0.410418197460951));
#22510=CARTESIAN_POINT('Ctrl Pts',(3.646,1.89157464001029,-0.402907279500277));
#22511=CARTESIAN_POINT('Ctrl Pts',(3.646,1.89970424140916,-0.328705005123505));
#22512=CARTESIAN_POINT('Ctrl Pts',(3.646,1.90312005139857,-0.253949891494488));
#22513=CARTESIAN_POINT('Ctrl Pts',(3.646,1.90195657636727,-0.179041257804402));
#22514=CARTESIAN_POINT('Ctrl Pts',(3.646,1.90168714256733,-0.161694157711369));
#22515=CARTESIAN_POINT('Ctrl Pts',(3.646,1.9011718953687,-0.144338912994997));
#22516=CARTESIAN_POINT('Ctrl Pts',(3.646,1.90041209170278,-0.126980670648089));
#22517=CARTESIAN_POINT('Ctrl Pts',(3.646,1.89981112648655,-0.113251202979906));
#22518=CARTESIAN_POINT('Ctrl Pts',(3.646,1.89905757038205,-0.099529250292602));
#22519=CARTESIAN_POINT('Ctrl Pts',(3.646,1.89815266633269,-0.0858180755197819));
#22520=CARTESIAN_POINT('Ctrl Pts',(3.646,1.89346054585753,-0.0147227102867202));
#22521=CARTESIAN_POINT('Ctrl Pts',(3.646,1.88470293100181,0.0560916653141868));
#22522=CARTESIAN_POINT('Ctrl Pts',(3.646,1.87201708655583,0.126279358269305));
#22523=CARTESIAN_POINT('Ctrl Pts',(3.646,1.86260788358229,0.178338190621555));
#22524=CARTESIAN_POINT('Ctrl Pts',(3.646,1.851036486259,0.230052140379478));
#22525=CARTESIAN_POINT('Ctrl Pts',(3.646,1.83734247846642,0.281271602238531));
#22526=CARTESIAN_POINT('Ctrl Pts',(3.646,1.83198896790198,0.301295245741617));
#22527=CARTESIAN_POINT('Ctrl Pts',(3.646,1.82631091397735,0.321243214387335));
#22528=CARTESIAN_POINT('Ctrl Pts',(3.646,1.82031016933083,0.341106135959376));
#22529=CARTESIAN_POINT('Ctrl Pts',(3.646,1.81552257077984,0.356953451607448));
#22530=CARTESIAN_POINT('Ctrl Pts',(3.646,1.81052809968397,0.372750635976576));
#22531=CARTESIAN_POINT('Ctrl Pts',(3.646,1.80533673969134,0.388466303818269));
#22532=CARTESIAN_POINT('Ctrl Pts',(3.646,1.78349989834249,0.454572400455262));
#22533=CARTESIAN_POINT('Ctrl Pts',(3.646,1.75815877282522,0.519325115466895));
#22534=CARTESIAN_POINT('Ctrl Pts',(3.646,1.72944007783936,0.582403703796427));
#22535=CARTESIAN_POINT('Ctrl Pts',(3.646,1.7013580179239,0.644083968088538));
#22536=CARTESIAN_POINT('Ctrl Pts',(3.646,1.67004582822095,0.704164273758678));
#22537=CARTESIAN_POINT('Ctrl Pts',(3.646,1.63558364196677,0.762314720566202));
#22538=CARTESIAN_POINT('Ctrl Pts',(3.646,1.6107204306916,0.804268148420632));
#22539=CARTESIAN_POINT('Ctrl Pts',(3.646,1.58421680890061,0.845216482048597));
#22540=CARTESIAN_POINT('Ctrl Pts',(3.646,1.55609275564537,0.885022483158703));
#22541=CARTESIAN_POINT('Ctrl Pts',(3.646,1.54206067170508,0.904883103668667));
#22542=CARTESIAN_POINT('Ctrl Pts',(3.646,1.52762508230321,0.924459162026505));
#22543=CARTESIAN_POINT('Ctrl Pts',(3.646,1.51278780298836,0.943732354103002));
#22544=CARTESIAN_POINT('Ctrl Pts',(3.646,1.5040149219818,0.955128070063854));
#22545=CARTESIAN_POINT('Ctrl Pts',(3.646,1.49510160076979,0.966417886209972));
#22546=CARTESIAN_POINT('Ctrl Pts',(3.646,1.48604814989002,0.977597866731241));
#22547=CARTESIAN_POINT('Ctrl Pts',(3.646,1.47811974575181,0.987388542685312));
#22548=CARTESIAN_POINT('Ctrl Pts',(3.646,1.4700886402459,0.997089004542171));
#22549=CARTESIAN_POINT('Ctrl Pts',(3.646,1.46196065824995,1.00669091177099));
#22550=CARTESIAN_POINT('Ctrl Pts',(3.646,1.4198448625495,1.05644397020358));
#22551=CARTESIAN_POINT('Ctrl Pts',(3.646,1.37508773873266,1.10360721210258));
#22552=CARTESIAN_POINT('Ctrl Pts',(3.646,1.32776700421932,1.14788094866693));
#22553=CARTESIAN_POINT('Ctrl Pts',(3.646,1.30623682000847,1.16802479710327));
#22554=CARTESIAN_POINT('Ctrl Pts',(3.646,1.28417551167546,1.18756994121615));
#22555=CARTESIAN_POINT('Ctrl Pts',(3.646,1.26158843649361,1.20648512205778));
#22556=CARTESIAN_POINT('Ctrl Pts',(3.646,1.21030221098365,1.24943394223017));
#22557=CARTESIAN_POINT('Ctrl Pts',(3.646,1.15630601551353,1.28913837264243));
#22558=CARTESIAN_POINT('Ctrl Pts',(3.646,1.09994475084755,1.32549904345976));
#22559=CARTESIAN_POINT('Ctrl Pts',(3.646,1.07528669755618,1.34140683694234));
#22560=CARTESIAN_POINT('Ctrl Pts',(3.646,1.05017579133236,1.35667393594728));
#22561=CARTESIAN_POINT('Ctrl Pts',(3.646,1.0246405521453,1.37128880994725));
#22562=CARTESIAN_POINT('Ctrl Pts',(3.646,1.00962813908413,1.37988103513524));
#22563=CARTESIAN_POINT('Ctrl Pts',(3.646,0.99446905996368,1.38824778952788));
#22564=CARTESIAN_POINT('Ctrl Pts',(3.646,0.97916913378863,1.39638640825901));
#22565=CARTESIAN_POINT('Ctrl Pts',(3.646,0.968921661455415,1.40183743261845));
#22566=CARTESIAN_POINT('Ctrl Pts',(3.646,0.958610248820093,1.40718638752318));
#22567=CARTESIAN_POINT('Ctrl Pts',(3.646,0.948251329433642,1.41242531107771));
#22568=CARTESIAN_POINT('Ctrl Pts',(3.646,0.890485005097459,1.44164007237986));
#22569=CARTESIAN_POINT('Ctrl Pts',(3.646,0.831136756612497,1.46749477000214));
#22570=CARTESIAN_POINT('Ctrl Pts',(3.646,0.770533170445064,1.48993478777504));
#22571=CARTESIAN_POINT('Ctrl Pts',(3.646,0.71007092264702,1.51232247142513));
#22572=CARTESIAN_POINT('Ctrl Pts',(3.646,0.648358055128917,1.53131144137255));
#22573=CARTESIAN_POINT('Ctrl Pts',(3.646,0.585713135036152,1.54679634298933));
#22574=CARTESIAN_POINT('Ctrl Pts',(3.646,0.524282126391685,1.5619811835745));
#22575=CARTESIAN_POINT('Ctrl Pts',(3.646,0.461953855213984,1.57379634993966));
#22576=CARTESIAN_POINT('Ctrl Pts',(3.646,0.399038762127085,1.58209375444539));
#22577=CARTESIAN_POINT('Ctrl Pts',(3.646,0.385552018248948,1.58387242096135));
#22578=CARTESIAN_POINT('Ctrl Pts',(3.646,0.372038376342684,1.5854892608117));
#22579=CARTESIAN_POINT('Ctrl Pts',(3.646,0.358501021440916,1.58694252210702));
#22580=CARTESIAN_POINT('Ctrl Pts',(3.646,0.347711851978039,1.58810076036721));
#22581=CARTESIAN_POINT('Ctrl Pts',(3.646,0.336912962054473,1.58915446959528));
#22582=CARTESIAN_POINT('Ctrl Pts',(3.646,0.326113495044186,1.59010251750235));
#22583=CARTESIAN_POINT('Ctrl Pts',(3.646,0.264279472447157,1.59553071276911));
#22584=CARTESIAN_POINT('Ctrl Pts',(3.646,0.202349440359449,1.59750742949326));
#22585=CARTESIAN_POINT('Ctrl Pts',(3.646,0.140612115364729,1.59594625728721));
#22586=CARTESIAN_POINT('Ctrl Pts',(3.646,0.0799615604267115,1.5944125665959));
#22587=CARTESIAN_POINT('Ctrl Pts',(3.646,0.0194961016000075,1.58946431823579));
#22588=CARTESIAN_POINT('Ctrl Pts',(3.646,-0.0404959561586677,1.5809719777752));
#22589=CARTESIAN_POINT('Ctrl Pts',(3.646,-0.0985852921086698,1.57274898232468));
#22590=CARTESIAN_POINT('Ctrl Pts',(3.646,-0.156231425499309,1.561202914565));
#22591=CARTESIAN_POINT('Ctrl Pts',(3.646,-0.213147860982218,1.54617388631109));
#22592=CARTESIAN_POINT('Ctrl Pts',(3.646,-0.227131809032557,1.54248136501093));
#22593=CARTESIAN_POINT('Ctrl Pts',(3.646,-0.24107156350228,1.53857839846659));
#22594=CARTESIAN_POINT('Ctrl Pts',(3.646,-0.254962570226321,1.53446223081039));
#22595=CARTESIAN_POINT('Ctrl Pts',(0.178525917727935,-0.685825729128712,
1.39614588036676));
#22596=CARTESIAN_POINT('Ctrl Pts',(0.214645439418269,-1.13846748842057,
1.17379564536202));
#22597=CARTESIAN_POINT('Ctrl Pts',(0.286884482798937,-1.80431739237854,
0.259468333747379));
#22598=CARTESIAN_POINT('Ctrl Pts',(0.395243047869939,-1.22944579344352,
-1.34783917131191));
#22599=CARTESIAN_POINT('Ctrl Pts',(0.503601612940941,0.420984007196011,
-1.77351976747628));
#22600=CARTESIAN_POINT('Ctrl Pts',(0.611960178011943,1.70289301291901,-0.651599460365548));
#22601=CARTESIAN_POINT('Ctrl Pts',(0.720318743082945,1.49728705490344,1.04067255962924));
#22602=CARTESIAN_POINT('Ctrl Pts',(0.828677308153947,-0.0167383245662881,
1.8231374532372));
#22603=CARTESIAN_POINT('Ctrl Pts',(0.937035873224949,-1.51604025138297,
1.0129450519225));
#22604=CARTESIAN_POINT('Ctrl Pts',(1.04539443829595,-1.69077758585837,-0.682438578679264));
#22605=CARTESIAN_POINT('Ctrl Pts',(1.15375300336695,-0.388197806685981,
-1.78147566906063));
#22606=CARTESIAN_POINT('Ctrl Pts',(1.26211156843795,1.2535495552727,-1.3240166887812));
#22607=CARTESIAN_POINT('Ctrl Pts',(1.37047013350896,1.8000352141881,0.290301877450055));
#22608=CARTESIAN_POINT('Ctrl Pts',(1.47882869857996,0.773764763351813,1.65096279999703));
#22609=CARTESIAN_POINT('Ctrl Pts',(1.58718726365096,-0.928568406390638,
1.56912687330982));
#22610=CARTESIAN_POINT('Ctrl Pts',(1.69554582872196,-1.81958063721889,0.11628815110578));
#22611=CARTESIAN_POINT('Ctrl Pts',(1.80390439379297,-1.1207626488587,-1.43815386147426));
#22612=CARTESIAN_POINT('Ctrl Pts',(1.91226295886397,0.557303862904986,-1.73603266764626));
#22613=CARTESIAN_POINT('Ctrl Pts',(2.02062152393497,1.74843472771405,-0.517079730093531));
#22614=CARTESIAN_POINT('Ctrl Pts',(2.12898008900597,1.41189906885343,1.15366271015419));
#22615=CARTESIAN_POINT('Ctrl Pts',(2.23733865407697,-0.158262365011203,
1.81641169719614));
#22616=CARTESIAN_POINT('Ctrl Pts',(2.34569721914797,-1.59014198076045,0.892097840487327));
#22617=CARTESIAN_POINT('Ctrl Pts',(2.45405578421898,-1.63266518861614,-0.811668857508549));
#22618=CARTESIAN_POINT('Ctrl Pts',(2.56241434928998,-0.248663526484289,
-1.80625943050602));
#22619=CARTESIAN_POINT('Ctrl Pts',(2.67077291436098,1.35258575494928,-1.22264666689896));
#22620=CARTESIAN_POINT('Ctrl Pts',(2.77913147943198,1.77206945169698,0.429209875088153));
#22621=CARTESIAN_POINT('Ctrl Pts',(2.88749004450298,0.643168985847878,1.70609770460869));
#22622=CARTESIAN_POINT('Ctrl Pts',(2.99584860957399,-1.04756297297815,1.4922205475568));
#22623=CARTESIAN_POINT('Ctrl Pts',(3.10420717464499,-1.82324663843674,-0.0252902466545985));
#22624=CARTESIAN_POINT('Ctrl Pts',(3.21256573971599,-1.00543213394195,-1.52103014244754));
#22625=CARTESIAN_POINT('Ctrl Pts',(3.320924304787,0.68997158388018,-1.68716896408801));
#22626=CARTESIAN_POINT('Ctrl Pts',(3.429282869858,1.78424156303041,-0.380380645529688));
#22627=CARTESIAN_POINT('Ctrl Pts',(3.53764143492899,1.31614849123568,1.26120506567147));
#22628=CARTESIAN_POINT('Ctrl Pts',(3.60988047830967,0.242522465892156,1.61712315325676));
#22629=CARTESIAN_POINT('Ctrl Pts',(3.646,-0.254962570226321,1.53446223081039));
#22630=CARTESIAN_POINT('Ctrl Pts',(0.25521727848529,-0.744392439309316,
1.51537102412035));
#22631=CARTESIAN_POINT('Ctrl Pts',(0.291336800175624,-1.23568795218047,
1.27403298912647));
#22632=CARTESIAN_POINT('Ctrl Pts',(0.363575843556292,-1.95839871261059,
0.281625867444654));
#22633=CARTESIAN_POINT('Ctrl Pts',(0.471934408627294,-1.33443543207789,
-1.46293911983174));
#22634=CARTESIAN_POINT('Ctrl Pts',(0.580292973698296,0.456934318321611,
-1.92497109659646));
#22635=CARTESIAN_POINT('Ctrl Pts',(0.688651538769298,1.84831310627553,-0.707243387282011));
#22636=CARTESIAN_POINT('Ctrl Pts',(0.7970101038403,1.62514924099131,1.12954173674534));
#22637=CARTESIAN_POINT('Ctrl Pts',(0.905368668911302,-0.0181677089742313,
1.97882592963601));
#22638=CARTESIAN_POINT('Ctrl Pts',(1.0137272339823,-1.64550388369329,1.09944641336922));
#22639=CARTESIAN_POINT('Ctrl Pts',(1.12208579905331,-1.8351630713324,-0.740716040075106));
#22640=CARTESIAN_POINT('Ctrl Pts',(1.23044436412431,-0.421348310482051,
-1.93360639961257));
#22641=CARTESIAN_POINT('Ctrl Pts',(1.33880292919531,1.36059755651049,-1.43708229479842));
#22642=CARTESIAN_POINT('Ctrl Pts',(1.44716149426631,1.95375085392965,0.315092469577743));
#22643=CARTESIAN_POINT('Ctrl Pts',(1.55552005933731,0.83984110712031,1.79194826572055));
#22644=CARTESIAN_POINT('Ctrl Pts',(1.66387862440832,-1.00786434766282,1.70312388584898));
#22645=CARTESIAN_POINT('Ctrl Pts',(1.77223718947932,-1.9749653760878,0.126218683242426));
#22646=CARTESIAN_POINT('Ctrl Pts',(1.88059575455032,-1.21647119178599,-1.56096631487563));
#22647=CARTESIAN_POINT('Ctrl Pts',(1.98895431962132,0.604895331750507,-1.88428275187577));
#22648=CARTESIAN_POINT('Ctrl Pts',(2.09731288469232,1.89774389711168,-0.561236222634466));
#22649=CARTESIAN_POINT('Ctrl Pts',(2.20567144976333,1.53246947042594,1.25218078365605));
#22650=CARTESIAN_POINT('Ctrl Pts',(2.31403001483433,-0.171777323214773,
1.97152582155758));
#22651=CARTESIAN_POINT('Ctrl Pts',(2.42238857990533,-1.72593359746098,0.96827934470552));
#22652=CARTESIAN_POINT('Ctrl Pts',(2.53074714497633,-1.77208811321992,-0.880982055776449));
#22653=CARTESIAN_POINT('Ctrl Pts',(2.63910571004733,-0.269898373865409,
-1.96050659284538));
#22654=CARTESIAN_POINT('Ctrl Pts',(2.74746427511834,1.46809104228396,-1.32705568795526));
#22655=CARTESIAN_POINT('Ctrl Pts',(2.85582284018934,1.92339692978575,0.465862641663236));
#22656=CARTESIAN_POINT('Ctrl Pts',(2.96418140526034,0.698092984746491,1.8517914655187));
#22657=CARTESIAN_POINT('Ctrl Pts',(3.07253997033134,-1.13702056319175,1.61965007465449));
#22658=CARTESIAN_POINT('Ctrl Pts',(3.18089853540234,-1.97894443880469,-0.0274499302058373));
#22659=CARTESIAN_POINT('Ctrl Pts',(3.28925710047335,-1.09129192294352,-1.65091989103114));
#22660=CARTESIAN_POINT('Ctrl Pts',(3.39761566554435,0.748892333087561,-1.83124628803295));
#22661=CARTESIAN_POINT('Ctrl Pts',(3.50597423061535,1.93660848960656,-0.412863595758679));
#22662=CARTESIAN_POINT('Ctrl Pts',(3.61433279568635,1.42854218538706,1.36890681616329));
#22663=CARTESIAN_POINT('Ctrl Pts',(3.68657183906702,0.263232891834088,1.75521885165445));
#22664=CARTESIAN_POINT('Ctrl Pts',(3.72269136075735,-0.276735330161002,
1.66549902476259));
#22665=CARTESIAN_POINT('Ctrl Pts',(0.331908639242645,-0.80295914948992,
1.63459616787395));
#22666=CARTESIAN_POINT('Ctrl Pts',(0.368028160932979,-1.33290841594038,
1.37427033289091));
#22667=CARTESIAN_POINT('Ctrl Pts',(0.440267204313648,-2.11248003284263,
0.303783401141929));
#22668=CARTESIAN_POINT('Ctrl Pts',(0.548625769384649,-1.43942507071225,
-1.57803906835158));
#22669=CARTESIAN_POINT('Ctrl Pts',(0.656984334455651,0.492884629447209,
-2.07642242571663));
#22670=CARTESIAN_POINT('Ctrl Pts',(0.765342899526654,1.99373319963206,-0.762887314198474));
#22671=CARTESIAN_POINT('Ctrl Pts',(0.873701464597655,1.75301142707918,1.21841091386143));
#22672=CARTESIAN_POINT('Ctrl Pts',(0.982060029668658,-0.0195970933821744,
2.13451440603482));
#22673=CARTESIAN_POINT('Ctrl Pts',(1.09041859473966,-1.77496751600361,1.18594777481594));
#22674=CARTESIAN_POINT('Ctrl Pts',(1.19877715981066,-1.97954855680643,-0.798993501470944));
#22675=CARTESIAN_POINT('Ctrl Pts',(1.30713572488166,-0.454498814278123,
-2.08573713016452));
#22676=CARTESIAN_POINT('Ctrl Pts',(1.41549428995266,1.46764555774828,-1.55014790081563));
#22677=CARTESIAN_POINT('Ctrl Pts',(1.52385285502367,2.10746649367121,0.339883061705427));
#22678=CARTESIAN_POINT('Ctrl Pts',(1.63221142009467,0.905917450888808,1.93293373144407));
#22679=CARTESIAN_POINT('Ctrl Pts',(1.74056998516567,-1.08716028893501,1.83712089838813));
#22680=CARTESIAN_POINT('Ctrl Pts',(1.84892855023667,-2.1303501149567,0.136149215379072));
#22681=CARTESIAN_POINT('Ctrl Pts',(1.95728711530768,-1.31217973471328,-1.683778768277));
#22682=CARTESIAN_POINT('Ctrl Pts',(2.06564568037868,0.652486800596032,-2.03253283610529));
#22683=CARTESIAN_POINT('Ctrl Pts',(2.17400424544968,2.04705306650931,-0.605392715175402));
#22684=CARTESIAN_POINT('Ctrl Pts',(2.28236281052068,1.65303987199845,1.35069885715791));
#22685=CARTESIAN_POINT('Ctrl Pts',(2.39072137559168,-0.185292281418345,
2.12663994591902));
#22686=CARTESIAN_POINT('Ctrl Pts',(2.49907994066268,-1.86172521416151,1.04446084892372));
#22687=CARTESIAN_POINT('Ctrl Pts',(2.60743850573369,-1.9115110378237,-0.95029525404435));
#22688=CARTESIAN_POINT('Ctrl Pts',(2.71579707080469,-0.291133221246527,
-2.11475375518475));
#22689=CARTESIAN_POINT('Ctrl Pts',(2.8241556358757,1.58359632961863,-1.43146470901156));
#22690=CARTESIAN_POINT('Ctrl Pts',(2.93251420094669,2.07472440787453,0.502515408238319));
#22691=CARTESIAN_POINT('Ctrl Pts',(3.04087276601769,0.753016983645105,1.99748522642871));
#22692=CARTESIAN_POINT('Ctrl Pts',(3.1492313310887,-1.22647815340536,1.74707960175219));
#22693=CARTESIAN_POINT('Ctrl Pts',(3.2575898961597,-2.13464223917264,-0.029609613757076));
#22694=CARTESIAN_POINT('Ctrl Pts',(3.3659484612307,-1.1771517119451,-1.78080963961473));
#22695=CARTESIAN_POINT('Ctrl Pts',(3.4743070263017,0.807813082294942,-1.9753236119779));
#22696=CARTESIAN_POINT('Ctrl Pts',(3.58266559137271,2.08897541618271,-0.44534654598767));
#22697=CARTESIAN_POINT('Ctrl Pts',(3.69102415644371,1.54093587953844,1.47660856665511));
#22698=CARTESIAN_POINT('Ctrl Pts',(3.76326319982438,0.283943317776021,1.89331455005214));
#22699=CARTESIAN_POINT('Ctrl Pts',(3.79938272151471,-0.298508090095682,
1.79653581871479));
#22700=CARTESIAN_POINT('Ctrl Pts',(0.408600000000001,-0.861525859670525,
1.75382131162755));
#22701=CARTESIAN_POINT('Ctrl Pts',(0.444719521690335,-1.43012887970028,
1.47450767665535));
#22702=CARTESIAN_POINT('Ctrl Pts',(0.516958565071002,-2.26656135307468,
0.325940934839204));
#22703=CARTESIAN_POINT('Ctrl Pts',(0.625317130142005,-1.54441470934661,
-1.69313901687141));
#22704=CARTESIAN_POINT('Ctrl Pts',(0.733675695213006,0.528834940572807,
-2.22787375483681));
#22705=CARTESIAN_POINT('Ctrl Pts',(0.84203426028401,2.13915329298858,-0.818531241114937));
#22706=CARTESIAN_POINT('Ctrl Pts',(0.950392825355009,1.88087361316704,1.30728009097753));
#22707=CARTESIAN_POINT('Ctrl Pts',(1.05875139042601,-0.0210264777901153,
2.29020288243362));
#22708=CARTESIAN_POINT('Ctrl Pts',(1.16710995549701,-1.90443114831393,1.27244913626267));
#22709=CARTESIAN_POINT('Ctrl Pts',(1.27546852056802,-2.12393404228046,-0.857270962866784));
#22710=CARTESIAN_POINT('Ctrl Pts',(1.38382708563902,-0.487649318074194,
-2.23786786071647));
#22711=CARTESIAN_POINT('Ctrl Pts',(1.49218565071002,1.57469355898608,-1.66321350683284));
#22712=CARTESIAN_POINT('Ctrl Pts',(1.60054421578102,2.26118213341276,0.364673653833113));
#22713=CARTESIAN_POINT('Ctrl Pts',(1.70890278085203,0.971993794657307,2.07391919716759));
#22714=CARTESIAN_POINT('Ctrl Pts',(1.81726134592303,-1.1664562302072,1.97111791092728));
#22715=CARTESIAN_POINT('Ctrl Pts',(1.92561991099403,-2.2857348538256,0.146079747515718));
#22716=CARTESIAN_POINT('Ctrl Pts',(2.03397847606503,-1.40788827764057,-1.80659122167837));
#22717=CARTESIAN_POINT('Ctrl Pts',(2.14233704113603,0.700078269441555,-2.1807829203348));
#22718=CARTESIAN_POINT('Ctrl Pts',(2.25069560620703,2.19636223590694,-0.649549207716336));
#22719=CARTESIAN_POINT('Ctrl Pts',(2.35905417127804,1.77361027357095,1.44921693065978));
#22720=CARTESIAN_POINT('Ctrl Pts',(2.46741273634904,-0.198807239621914,
2.28175407028046));
#22721=CARTESIAN_POINT('Ctrl Pts',(2.57577130142004,-1.99751683086205,1.12064235314191));
#22722=CARTESIAN_POINT('Ctrl Pts',(2.68412986649105,-2.05093396242748,-1.01960845231225));
#22723=CARTESIAN_POINT('Ctrl Pts',(2.79248843156204,-0.312368068627645,
-2.26900091752411));
#22724=CARTESIAN_POINT('Ctrl Pts',(2.90084699663305,1.69910161695331,-1.53587373006786));
#22725=CARTESIAN_POINT('Ctrl Pts',(3.00920556170405,2.2260518859633,0.539168174813403));
#22726=CARTESIAN_POINT('Ctrl Pts',(3.11756412677505,0.807940982543718,2.14317898733871));
#22727=CARTESIAN_POINT('Ctrl Pts',(3.22592269184605,-1.31593574361896,1.87450912884988));
#22728=CARTESIAN_POINT('Ctrl Pts',(3.33428125691705,-2.29034003954059,-0.0317692973083151));
#22729=CARTESIAN_POINT('Ctrl Pts',(3.44263982198806,-1.26301150094668,-1.91069938819832));
#22730=CARTESIAN_POINT('Ctrl Pts',(3.55099838705906,0.866733831502324,-2.11940093592284));
#22731=CARTESIAN_POINT('Ctrl Pts',(3.65935695213006,2.24134234275887,-0.477829496216659));
#22732=CARTESIAN_POINT('Ctrl Pts',(3.76771551720106,1.65332957368982,1.58431031714693));
#22733=CARTESIAN_POINT('Ctrl Pts',(3.83995456058173,0.304653743717953,2.03141024844982));
#22734=CARTESIAN_POINT('Ctrl Pts',(3.87607408227206,-0.320280850030362,
1.92757261266699));
#22735=CARTESIAN_POINT('Ctrl Pts',(3.33273030787577,-1.95689202958038,-0.000120183693368507));
#22736=CARTESIAN_POINT('Ctrl Pts',(3.33324729088953,-1.95690205649134,-0.00915092760564931));
#22737=CARTESIAN_POINT('Ctrl Pts',(3.33376427390329,-1.95684415228561,-0.0181815514118841));
#22738=CARTESIAN_POINT('Ctrl Pts',(3.33428125691705,-1.95671790045467,-0.0272112414302843));
#22739=CARTESIAN_POINT('Ctrl Pts',(3.37040077860739,-1.94789719334262,-0.658079327604984));
#22740=CARTESIAN_POINT('Ctrl Pts',(3.40652030029772,-1.60545434714465,-1.28438935790166));
#22741=CARTESIAN_POINT('Ctrl Pts',(3.44263982198806,-1.0792753686375,-1.63232796433741));
#22742=CARTESIAN_POINT('Ctrl Pts',(3.47875934367839,-0.553096390130347,
-1.98026657077316));
#22743=CARTESIAN_POINT('Ctrl Pts',(3.51487886536873,0.156818720685984,-2.049833753348));
#22744=CARTESIAN_POINT('Ctrl Pts',(3.55099838705906,0.740877694636909,-1.81102210468439));
#22745=CARTESIAN_POINT('Ctrl Pts',(3.58266559137271,1.2529419190165,-1.60164786834911));
#22746=CARTESIAN_POINT('Ctrl Pts',(3.61433279568635,1.668265301163,-1.1552345125566));
#22747=CARTESIAN_POINT('Ctrl Pts',(3.646,1.85122479320614,-0.632364557278426));
#22748=CARTESIAN_POINT('',(0.408600000000001,-0.905313301390919,-1.26710934922959));
#22749=CARTESIAN_POINT('Ctrl Pts',(0.408600000000001,-0.905313301390914,
-1.26710934922959));
#22750=CARTESIAN_POINT('Ctrl Pts',(0.408600000000001,-0.960992218100913,
-1.23747014056059));
#22751=CARTESIAN_POINT('Ctrl Pts',(0.4086,-1.0146111721236,-1.20440946055571));
#22752=CARTESIAN_POINT('Ctrl Pts',(0.4086,-1.06580548946931,-1.16801868547721));
#22753=CARTESIAN_POINT('Ctrl Pts',(0.408600000000001,-1.11460808220303,
-1.13332803488357));
#22754=CARTESIAN_POINT('Ctrl Pts',(0.408600000000001,-1.16120868065023,
-1.09561111056787));
#22755=CARTESIAN_POINT('Ctrl Pts',(0.408600000000001,-1.20553237586123,
-1.05517990554672));
#22756=CARTESIAN_POINT('Ctrl Pts',(0.408600000000001,-1.21581352958369,
-1.04580163886502));
#22757=CARTESIAN_POINT('Ctrl Pts',(0.408600000000001,-1.22597208544125,
-1.03627713244074));
#22758=CARTESIAN_POINT('Ctrl Pts',(0.408600000000001,-1.23600692964817,
-1.02660993024093));
#22759=CARTESIAN_POINT('Ctrl Pts',(0.408600000000001,-1.24536959860237,
-1.01759027711592));
#22760=CARTESIAN_POINT('Ctrl Pts',(0.408600000000001,-1.25462100326372,
-1.0084497486066));
#22761=CARTESIAN_POINT('Ctrl Pts',(0.408600000000001,-1.2637547881083,-0.999197404829853));
#22762=CARTESIAN_POINT('Ctrl Pts',(0.408600000000001,-1.30741516684387,
-0.954970302882759));
#22763=CARTESIAN_POINT('Ctrl Pts',(0.408600000000001,-1.34842999904488,
-0.908153772000464));
#22764=CARTESIAN_POINT('Ctrl Pts',(0.408600000000001,-1.38672592196133,
-0.859098143986562));
#22765=CARTESIAN_POINT('Ctrl Pts',(0.408600000000001,-1.41723561179862,
-0.820016385890729));
#22766=CARTESIAN_POINT('Ctrl Pts',(0.408600000000001,-1.44601935179638,
-0.779512241439089));
#22767=CARTESIAN_POINT('Ctrl Pts',(0.408600000000001,-1.47302824589713,
-0.737742377449649));
#22768=CARTESIAN_POINT('Ctrl Pts',(0.408600000000001,-1.48400331805306,
-0.720769180786444));
#22769=CARTESIAN_POINT('Ctrl Pts',(0.408600000000001,-1.4946851893039,-0.703586803249634));
#22770=CARTESIAN_POINT('Ctrl Pts',(0.408600000000001,-1.50506997244662,
-0.686205058605768));
#22771=CARTESIAN_POINT('Ctrl Pts',(0.4086,-1.51138034557605,-0.675642941627891));
#22772=CARTESIAN_POINT('Ctrl Pts',(0.408600000000001,-1.51757627535282,
-0.665015095569133));
#22773=CARTESIAN_POINT('Ctrl Pts',(0.408600000000001,-1.52365605181011,
-0.654326316602663));
#22774=CARTESIAN_POINT('Ctrl Pts',(0.408600000000001,-1.55558277317524,
-0.598196346990612));
#22775=CARTESIAN_POINT('Ctrl Pts',(0.408600000000001,-1.5843201739237,-0.540370467208204));
#22776=CARTESIAN_POINT('Ctrl Pts',(0.408600000000001,-1.60979082996186,
-0.481204228927061));
#22777=CARTESIAN_POINT('Ctrl Pts',(0.408600000000001,-1.63580594349255,
-0.420773260688075));
#22778=CARTESIAN_POINT('Ctrl Pts',(0.408600000000001,-1.65841388453419,
-0.358943232312242));
#22779=CARTESIAN_POINT('Ctrl Pts',(0.408600000000001,-1.67749735979264,
-0.296051832948879));
#22780=CARTESIAN_POINT('Ctrl Pts',(0.408600000000001,-1.69091866366144,
-0.251820655442808));
#22781=CARTESIAN_POINT('Ctrl Pts',(0.408600000000001,-1.70259596991367,
-0.207063606073226));
#22782=CARTESIAN_POINT('Ctrl Pts',(0.408600000000001,-1.71247552643195,
-0.161889744563548));
#22783=CARTESIAN_POINT('Ctrl Pts',(0.408600000000001,-1.71825809865879,
-0.135449173424395));
#22784=CARTESIAN_POINT('Ctrl Pts',(0.408600000000001,-1.72342457757944,
-0.108865697407971));
#22785=CARTESIAN_POINT('Ctrl Pts',(0.408600000000001,-1.72796221803694,
-0.0821604924653415));
#22786=CARTESIAN_POINT('Ctrl Pts',(0.408600000000001,-1.72987457329142,
-0.0709057799176328));
#22787=CARTESIAN_POINT('Ctrl Pts',(0.408600000000001,-1.73167514932966,
-0.0596292516012904));
#22788=CARTESIAN_POINT('Ctrl Pts',(0.408600000000001,-1.73336096201533,
-0.0483474786684694));
#22789=CARTESIAN_POINT('Ctrl Pts',(0.408600000000001,-1.74338265810016,
0.0187195807926847));
#22790=CARTESIAN_POINT('Ctrl Pts',(0.408600000000001,-1.74937481327135,
0.0860982634108857));
#22791=CARTESIAN_POINT('Ctrl Pts',(0.408600000000001,-1.751230653984,0.153428852725802));
#22792=CARTESIAN_POINT('Ctrl Pts',(0.408600000000001,-1.75211859736995,
0.18564376807186));
#22793=CARTESIAN_POINT('Ctrl Pts',(0.408600000000001,-1.7520590352964,0.217848150864259));
#22794=CARTESIAN_POINT('Ctrl Pts',(0.408600000000001,-1.75103660889884,
0.250004695309369));
#22795=CARTESIAN_POINT('Ctrl Pts',(0.408600000000001,-1.74896620456347,
0.315121410985578));
#22796=CARTESIAN_POINT('Ctrl Pts',(0.408600000000001,-1.74295098459612,
0.380041655358923));
#22797=CARTESIAN_POINT('Ctrl Pts',(0.408600000000001,-1.73320278712455,
0.444532054942262));
#22798=CARTESIAN_POINT('Ctrl Pts',(0.408600000000001,-1.72818815850798,
0.47770694744813));
#22799=CARTESIAN_POINT('Ctrl Pts',(0.408600000000001,-1.72218484157449,
0.510768222096462));
#22800=CARTESIAN_POINT('Ctrl Pts',(0.408600000000001,-1.71521645115096,
0.54368436163359));
#22801=CARTESIAN_POINT('Ctrl Pts',(0.408600000000001,-1.71145543383829,
0.561450038230503));
#22802=CARTESIAN_POINT('Ctrl Pts',(0.408600000000001,-1.70741322783236,
0.579173434823943));
#22803=CARTESIAN_POINT('Ctrl Pts',(0.408600000000001,-1.70309313761823,
0.596849557588417));
#22804=CARTESIAN_POINT('Ctrl Pts',(0.408600000000001,-1.70043783745291,
0.607714009341151));
#22805=CARTESIAN_POINT('Ctrl Pts',(0.408600000000001,-1.69767778945195,
0.618559301444646));
#22806=CARTESIAN_POINT('Ctrl Pts',(0.408600000000001,-1.6948171819072,0.62937234343737));
#22807=CARTESIAN_POINT('Ctrl Pts',(0.408600000000001,-1.67749388530445,
0.694854074394054));
#22808=CARTESIAN_POINT('Ctrl Pts',(0.408600000000001,-1.65645882135167,
0.759270632936003));
#22809=CARTESIAN_POINT('Ctrl Pts',(0.408600000000001,-1.63197264004038,
0.822370777365584));
#22810=CARTESIAN_POINT('Ctrl Pts',(0.408600000000001,-1.60696675159071,
0.886810191282533));
#22811=CARTESIAN_POINT('Ctrl Pts',(0.408600000000001,-1.57836151994529,
0.94987758575432));
#22812=CARTESIAN_POINT('Ctrl Pts',(0.408600000000001,-1.5463793183319,1.01130823187454));
#22813=CARTESIAN_POINT('Ctrl Pts',(0.408600000000001,-1.51413756653462,
1.07323741576553));
#22814=CARTESIAN_POINT('Ctrl Pts',(0.408600000000001,-1.47846348459479,
1.13350415064642));
#22815=CARTESIAN_POINT('Ctrl Pts',(0.408600000000001,-1.43953335033057,
1.19182606932565));
#22816=CARTESIAN_POINT('Ctrl Pts',(0.408600000000001,-1.42970202868341,
1.20655454515683));
#22817=CARTESIAN_POINT('Ctrl Pts',(0.408600000000001,-1.41966281092328,
1.22115889316257));
#22818=CARTESIAN_POINT('Ctrl Pts',(0.408600000000001,-1.40941806125765,
1.23563433772608));
#22819=CARTESIAN_POINT('Ctrl Pts',(0.408600000000001,-1.401932841117,1.24621067123621));
#22820=CARTESIAN_POINT('Ctrl Pts',(0.408600000000001,-1.39433687267044,
1.25671941680317));
#22821=CARTESIAN_POINT('Ctrl Pts',(0.408600000000001,-1.38664260250637,
1.26714345780971));
#22822=CARTESIAN_POINT('Ctrl Pts',(0.408600000000001,-1.34381660554335,
1.32516324902697));
#22823=CARTESIAN_POINT('Ctrl Pts',(0.408600000000001,-1.2978752047385,1.38066675809276));
#22824=CARTESIAN_POINT('Ctrl Pts',(0.408600000000001,-1.24906366160572,
1.43337782873043));
#22825=CARTESIAN_POINT('Ctrl Pts',(0.408600000000001,-1.20010611167173,
1.48624657057286));
#22826=CARTESIAN_POINT('Ctrl Pts',(0.408600000000001,-1.14826078782103,
1.53630714398619));
#22827=CARTESIAN_POINT('Ctrl Pts',(0.408600000000001,-1.09372545966621,
1.58326466535508));
#22828=CARTESIAN_POINT('Ctrl Pts',(0.408600000000001,-1.04029917410998,
1.62926724809456));
#22829=CARTESIAN_POINT('Ctrl Pts',(0.408600000000001,-0.984290607373418,
1.67229256006689));
#22830=CARTESIAN_POINT('Ctrl Pts',(0.408600000000001,-0.925845826339396,
1.71203418993537));
#22831=CARTESIAN_POINT('Ctrl Pts',(0.408600000000001,-0.904722483940492,
1.72639776595277));
#22832=CARTESIAN_POINT('Ctrl Pts',(0.408600000000001,-0.883280563501835,
1.74033206113498));
#22833=CARTESIAN_POINT('Ctrl Pts',(0.408600000000001,-0.861525859670525,
1.75382131162755));
#22834=CARTESIAN_POINT('Ctrl Pts',(0.4086,-0.905313301390919,-1.26710934922959));
#22835=CARTESIAN_POINT('Ctrl Pts',(0.440267204313647,-0.544607602467862,
-1.52079487885496));
#22836=CARTESIAN_POINT('Ctrl Pts',(0.508053930317628,0.473656038592629,
-1.7274214708134));
#22837=CARTESIAN_POINT('Ctrl Pts',(0.611960178011943,1.70289301291901,-0.651599460365548));
#22838=CARTESIAN_POINT('Ctrl Pts',(0.720318743082945,1.49728705490344,1.04067255962924));
#22839=CARTESIAN_POINT('Ctrl Pts',(0.828677308153947,-0.0167383245662881,
1.8231374532372));
#22840=CARTESIAN_POINT('Ctrl Pts',(0.922789802327533,-1.31892467005291,
1.11946232060462));
#22841=CARTESIAN_POINT('Ctrl Pts',(0.980782774810785,-1.55224362360984,
0.305528304683677));
#22842=CARTESIAN_POINT('Ctrl Pts',(1.0026562256037,-1.55363103362015,-0.000732727065787947));
#22843=CARTESIAN_POINT('Origin',(0.408600000000001,-2.59090492670967E-16,
0.));
#22844=CARTESIAN_POINT('',(0.408600000000001,-1.954,-2.39295984553393E-16));
#22845=CARTESIAN_POINT('Origin',(0.408600000000001,0.,0.));
#22846=CARTESIAN_POINT('Origin',(0.408600000000001,0.,0.));
#22847=CARTESIAN_POINT('',(0.408600000000001,0.90360677865021,-1.26612599672283));
#22848=CARTESIAN_POINT('Ctrl Pts',(0.408600000000001,0.863439746847563,
1.75538915071904));
#22849=CARTESIAN_POINT('Ctrl Pts',(0.408600000000001,0.923415504740013,
1.71873542152767));
#22850=CARTESIAN_POINT('Ctrl Pts',(0.4086,0.981160814141446,1.67880083042132));
#22851=CARTESIAN_POINT('Ctrl Pts',(0.408600000000001,1.03634589654915,1.63558766289775));
#22852=CARTESIAN_POINT('Ctrl Pts',(0.408600000000001,1.04229457843093,1.63092949486599));
#22853=CARTESIAN_POINT('Ctrl Pts',(0.408600000000001,1.04821347525907,1.6262331953884));
#22854=CARTESIAN_POINT('Ctrl Pts',(0.408600000000001,1.05410214691338,1.62149874228353));
#22855=CARTESIAN_POINT('Ctrl Pts',(0.408600000000001,1.11227764689379,1.5747260246523));
#22856=CARTESIAN_POINT('Ctrl Pts',(0.408600000000001,1.16750758234271,1.52423185527925));
#22857=CARTESIAN_POINT('Ctrl Pts',(0.408600000000001,1.21960503748186,1.4703938799972));
#22858=CARTESIAN_POINT('Ctrl Pts',(0.408600000000001,1.2316695712854,1.45792628304896));
#22859=CARTESIAN_POINT('Ctrl Pts',(0.408600000000001,1.2435658880977,1.44527926143554));
#22860=CARTESIAN_POINT('Ctrl Pts',(0.408600000000001,1.25529124126781,1.43245734592917));
#22861=CARTESIAN_POINT('Ctrl Pts',(0.408600000000001,1.26456542187468,1.42231583817185));
#22862=CARTESIAN_POINT('Ctrl Pts',(0.408600000000001,1.27372629854108,1.41207184696792));
#22863=CARTESIAN_POINT('Ctrl Pts',(0.408600000000001,1.28277244563777,1.40172855991044));
#22864=CARTESIAN_POINT('Ctrl Pts',(0.408600000000001,1.32967857189279,1.34809649717428));
#22865=CARTESIAN_POINT('Ctrl Pts',(0.408600000000001,1.37350887723089,1.29179113201222));
#22866=CARTESIAN_POINT('Ctrl Pts',(0.408600000000001,1.41411628391085,1.2331541048561));
#22867=CARTESIAN_POINT('Ctrl Pts',(0.408600000000001,1.44423515830919,1.18966250072767));
#22868=CARTESIAN_POINT('Ctrl Pts',(0.408600000000001,1.47258011132439,1.14488745049006));
#22869=CARTESIAN_POINT('Ctrl Pts',(0.408600000000001,1.4990734647959,1.0989628031704));
#22870=CARTESIAN_POINT('Ctrl Pts',(0.408600000000001,1.50943070523876,1.08100914490457));
#22871=CARTESIAN_POINT('Ctrl Pts',(0.4086,1.51950479225154,1.06287976458426));
#22872=CARTESIAN_POINT('Ctrl Pts',(0.4086,1.52929041576869,1.04458260423572));
#22873=CARTESIAN_POINT('Ctrl Pts',(0.4086,1.5370977611374,1.0299844286716));
#22874=CARTESIAN_POINT('Ctrl Pts',(0.408600000000001,1.54472327691443,1.01527558260098));
#22875=CARTESIAN_POINT('Ctrl Pts',(0.408600000000001,1.55215185596123,1.00048533214757));
#22876=CARTESIAN_POINT('Ctrl Pts',(0.408600000000001,1.58339919357882,0.938272095072908));
#22877=CARTESIAN_POINT('Ctrl Pts',(0.408600000000001,1.61121027972009,0.87454102427181));
#22878=CARTESIAN_POINT('Ctrl Pts',(0.408600000000001,1.63544819515225,0.809608649754739));
#22879=CARTESIAN_POINT('Ctrl Pts',(0.408600000000001,1.65914878364041,0.746115751931282));
#22880=CARTESIAN_POINT('Ctrl Pts',(0.408600000000001,1.67943295454144,0.681473222428096));
#22881=CARTESIAN_POINT('Ctrl Pts',(0.408600000000001,1.69612435377567,0.61597116125941));
#22882=CARTESIAN_POINT('Ctrl Pts',(0.408600000000001,1.70816660743026,0.568713742967382));
#22883=CARTESIAN_POINT('Ctrl Pts',(0.408600000000001,1.71833779962181,0.521008772156351));
#22884=CARTESIAN_POINT('Ctrl Pts',(0.408600000000001,1.72655511408715,0.472967494776519));
#22885=CARTESIAN_POINT('Ctrl Pts',(0.408600000000001,1.73065500678508,0.448998096603924));
#22886=CARTESIAN_POINT('Ctrl Pts',(0.408600000000001,1.73426828919771,0.424945031896326));
#22887=CARTESIAN_POINT('Ctrl Pts',(0.408600000000001,1.73738331488236,0.400822537981791));
#22888=CARTESIAN_POINT('Ctrl Pts',(0.408600000000001,1.73922474295558,0.386562675628391));
#22889=CARTESIAN_POINT('Ctrl Pts',(0.4086,1.74089203733157,0.372278557344402));
#22890=CARTESIAN_POINT('Ctrl Pts',(0.4086,1.74238263893657,0.357973186099987));
#22891=CARTESIAN_POINT('Ctrl Pts',(0.4086,1.74368858199248,0.345439991330694));
#22892=CARTESIAN_POINT('Ctrl Pts',(0.4086,1.74485804686663,0.332898075035613));
#22893=CARTESIAN_POINT('Ctrl Pts',(0.4086,1.74588926111498,0.320357474643566));
#22894=CARTESIAN_POINT('Ctrl Pts',(0.408600000000001,1.75123141071125,0.255391573107561));
#22895=CARTESIAN_POINT('Ctrl Pts',(0.408600000000001,1.7528745495965,0.19039258240519));
#22896=CARTESIAN_POINT('Ctrl Pts',(0.408600000000001,1.75066195802975,0.125627513646972));
#22897=CARTESIAN_POINT('Ctrl Pts',(0.408600000000001,1.74965524067005,0.0961597528542624));
#22898=CARTESIAN_POINT('Ctrl Pts',(0.408600000000001,1.74784961952587,0.0667405016615884));
#22899=CARTESIAN_POINT('Ctrl Pts',(0.408600000000001,1.74522680112737,0.0373956702521555));
#22900=CARTESIAN_POINT('Ctrl Pts',(0.408600000000001,1.73927155982219,-0.0292332477859586));
#22901=CARTESIAN_POINT('Ctrl Pts',(0.408600000000001,1.72910627580647,-0.0954804691698916));
#22902=CARTESIAN_POINT('Ctrl Pts',(0.408600000000001,1.71490485110609,-0.161032009093848));
#22903=CARTESIAN_POINT('Ctrl Pts',(0.408600000000001,1.70869172779967,-0.189710807810579));
#22904=CARTESIAN_POINT('Ctrl Pts',(0.408600000000001,1.70170546695327,-0.218256084698624));
#22905=CARTESIAN_POINT('Ctrl Pts',(0.408600000000001,1.69395810762654,-0.246639531074824));
#22906=CARTESIAN_POINT('Ctrl Pts',(0.408600000000001,1.68940335770069,-0.263326442682377));
#22907=CARTESIAN_POINT('Ctrl Pts',(0.408600000000001,1.68458551639814,-0.279957393553351));
#22908=CARTESIAN_POINT('Ctrl Pts',(0.408600000000001,1.67950681947972,-0.296526386780756));
#22909=CARTESIAN_POINT('Ctrl Pts',(0.408600000000001,1.67610525090757,-0.30762383314145));
#22910=CARTESIAN_POINT('Ctrl Pts',(0.408600000000001,1.67258631980131,-0.318694212312513));
#22911=CARTESIAN_POINT('Ctrl Pts',(0.408600000000001,1.6689560320264,-0.329720279574332));
#22912=CARTESIAN_POINT('Ctrl Pts',(0.408600000000001,1.6487117951502,-0.391206952615498));
#22913=CARTESIAN_POINT('Ctrl Pts',(0.408600000000001,1.62497416958449,-0.451433142841631));
#22914=CARTESIAN_POINT('Ctrl Pts',(0.408600000000001,1.59793571240631,-0.510129477960578));
#22915=CARTESIAN_POINT('Ctrl Pts',(0.408600000000001,1.57096028648465,-0.568688981908608));
#22916=CARTESIAN_POINT('Ctrl Pts',(0.408600000000001,1.54069864105028,-0.625726594487064));
#22917=CARTESIAN_POINT('Ctrl Pts',(0.408600000000001,1.50730181274075,-0.680942698188743));
#22918=CARTESIAN_POINT('Ctrl Pts',(0.408600000000001,1.4745521083011,-0.735088890149842));
#22919=CARTESIAN_POINT('Ctrl Pts',(0.408600000000001,1.43878678398125,-0.787484108438842));
#22920=CARTESIAN_POINT('Ctrl Pts',(0.408600000000001,1.40012093539101,-0.837804231710174));
#22921=CARTESIAN_POINT('Ctrl Pts',(0.408600000000001,1.39183183476257,-0.848591750428618));
#22922=CARTESIAN_POINT('Ctrl Pts',(0.408600000000001,1.38340935405792,-0.859283728160873));
#22923=CARTESIAN_POINT('Ctrl Pts',(0.408600000000001,1.37485451002538,-0.869876674256443));
#22924=CARTESIAN_POINT('Ctrl Pts',(0.408600000000001,1.36803642454044,-0.878319097255891));
#22925=CARTESIAN_POINT('Ctrl Pts',(0.408600000000001,1.36113760589381,-0.886694397807001));
#22926=CARTESIAN_POINT('Ctrl Pts',(0.408600000000001,1.35416372308826,-0.894995317810194));
#22927=CARTESIAN_POINT('Ctrl Pts',(0.408600000000001,1.31423588906621,-0.942520887906374));
#22928=CARTESIAN_POINT('Ctrl Pts',(0.408600000000001,1.27180173657993,-0.987671528671633));
#22929=CARTESIAN_POINT('Ctrl Pts',(0.408600000000001,1.22700455835745,-1.03018211725701));
#22930=CARTESIAN_POINT('Ctrl Pts',(0.408600000000001,1.1829959328827,-1.07194440332051));
#22931=CARTESIAN_POINT('Ctrl Pts',(0.408600000000001,1.13670602306087,-1.11115929871366));
#22932=CARTESIAN_POINT('Ctrl Pts',(0.408600000000001,1.08824736469086,-1.14753145000445));
#22933=CARTESIAN_POINT('Ctrl Pts',(0.408600000000001,1.04132560612878,-1.18275003340432));
#22934=CARTESIAN_POINT('Ctrl Pts',(0.408600000000001,0.992369867827824,
-1.2153036289198));
#22935=CARTESIAN_POINT('Ctrl Pts',(0.408600000000001,0.941469961039648,
-1.24487667804896));
#22936=CARTESIAN_POINT('Ctrl Pts',(0.408600000000001,0.928965840295594,
-1.2521416221405));
#22937=CARTESIAN_POINT('Ctrl Pts',(0.408600000000001,0.916344354236908,
-1.25922645029678));
#22938=CARTESIAN_POINT('Ctrl Pts',(0.408600000000001,0.903606778650211,
-1.26612599672283));
#22939=CARTESIAN_POINT('Origin',(0.408600000000001,0.,0.));
#22940=CARTESIAN_POINT('Origin',(-0.885456225603702,0.,0.));
#22941=CARTESIAN_POINT('Ctrl Pts',(0.408600000000001,0.903606778650209,
-1.26612599672283));
#22942=CARTESIAN_POINT('Ctrl Pts',(0.444719521690335,1.31409504259239,-0.973169388285302));
#22943=CARTESIAN_POINT('Ctrl Pts',(0.516958565071003,1.82250017258503,0.0372118057298887));
#22944=CARTESIAN_POINT('Ctrl Pts',(0.625317130142004,0.994051806197197,
1.52972919549323));
#22945=CARTESIAN_POINT('Ctrl Pts',(0.733675695213007,-0.703615338567789,
1.6815229998257));
#22946=CARTESIAN_POINT('Ctrl Pts',(0.813417909964438,-1.50026456430569,
0.713553299624354));
#22947=CARTESIAN_POINT('Ctrl Pts',(0.857040603025534,-1.55672331735519,
0.105986991352769));
#22948=CARTESIAN_POINT('Ctrl Pts',(0.864543774396297,-1.55583496332863,
0.00131431692112695));
#22949=CARTESIAN_POINT('Ctrl Pts',(0.178525917727935,1.13509973994375,-1.5904919303095));
#22950=CARTESIAN_POINT('Ctrl Pts',(0.214645439418269,1.65075005671844,-1.22248343600738));
#22951=CARTESIAN_POINT('Ctrl Pts',(0.286884482798937,2.28940233830353,0.046745013433751));
#22952=CARTESIAN_POINT('Ctrl Pts',(0.395243047869939,1.24871567297289,1.92162703181856));
#22953=CARTESIAN_POINT('Ctrl Pts',(0.50360161294094,-0.883872948609101,
2.11230854494337));
#22954=CARTESIAN_POINT('Ctrl Pts',(0.611960178011943,-2.2437405724288,0.459999581832252));
#22955=CARTESIAN_POINT('Ctrl Pts',(0.720318743082944,-1.64341174980208,
-1.59557661759511));
#22956=CARTESIAN_POINT('Ctrl Pts',(0.828677308153947,0.392945779374837,
-2.25633819105695));
#22957=CARTESIAN_POINT('Ctrl Pts',(0.937035873224949,2.08590841711691,-0.946028636835653));
#22958=CARTESIAN_POINT('Ctrl Pts',(1.04539443829595,1.95637548059159,1.19105133553842));
#22959=CARTESIAN_POINT('Ctrl Pts',(1.15375300336695,0.117472723211352,2.28736813879232));
#22960=CARTESIAN_POINT('Ctrl Pts',(1.26211156843795,-1.82406069577048,1.38518606320933));
#22961=CARTESIAN_POINT('Ctrl Pts',(1.37047013350896,-2.17185480860121,-0.727308039434555));
#22962=CARTESIAN_POINT('Ctrl Pts',(1.47882869857996,-0.622022654043615,
-2.20431378999848));
#22963=CARTESIAN_POINT('Ctrl Pts',(1.58718726365096,1.4712906547618,-1.75534285655934));
#22964=CARTESIAN_POINT('Ctrl Pts',(1.69554582872196,2.27908767273779,0.227335097164274));
#22965=CARTESIAN_POINT('Ctrl Pts',(1.80390439379297,1.09556770388087,2.01138046939323));
#22966=CARTESIAN_POINT('Ctrl Pts',(1.91226295886397,-1.04518727913395,2.03801522134292));
#22967=CARTESIAN_POINT('Ctrl Pts',(2.02062152393497,-2.27272600824398,0.283965628016336));
#22968=CARTESIAN_POINT('Ctrl Pts',(2.12898008900597,-1.51450731529388,-1.7181936614798));
#22969=CARTESIAN_POINT('Ctrl Pts',(2.23733865407697,0.56699002984457,-2.21910951530567));
#22970=CARTESIAN_POINT('Ctrl Pts',(2.34569721914798,2.15308520787897,-0.78111174266791));
#22971=CARTESIAN_POINT('Ctrl Pts',(2.45405578421898,1.85796319190442,1.33936666801838));
#22972=CARTESIAN_POINT('Ctrl Pts',(2.56241434928998,-0.0605379631590849,
2.28960105839));
#22973=CARTESIAN_POINT('Ctrl Pts',(2.67077291436098,-1.92611976024453,1.23932058494019));
#22974=CARTESIAN_POINT('Ctrl Pts',(2.77913147943199,-2.10883321481238,-0.893773336507565));
#22975=CARTESIAN_POINT('Ctrl Pts',(2.88749004450298,-0.448894737888299,
-2.24599145604085));
#22976=CARTESIAN_POINT('Ctrl Pts',(2.99584860957399,1.60308200591594,-1.63572506866501));
#22977=CARTESIAN_POINT('Ctrl Pts',(3.10420717464499,2.25472837895232,0.403567663658574));
#22978=CARTESIAN_POINT('Ctrl Pts',(3.21256573971599,0.93569695902205,2.0905603489318));
#22979=CARTESIAN_POINT('Ctrl Pts',(3.320924304787,-1.19965070554216,1.9503632900093));
#22980=CARTESIAN_POINT('Ctrl Pts',(3.42928286985799,-2.28920179463487,0.107221382123356));
#22981=CARTESIAN_POINT('Ctrl Pts',(3.537641434929,-1.37386884803431,-1.83194774797522));
#22982=CARTESIAN_POINT('Ctrl Pts',(3.60988047830967,0.0295369701314518,
-2.05391554560157));
#22983=CARTESIAN_POINT('Ctrl Pts',(3.646,0.629287956476874,-1.84989531266857));
#22984=CARTESIAN_POINT('Ctrl Pts',(0.25521727848529,1.05793541951257,-1.48236995244728));
#22985=CARTESIAN_POINT('Ctrl Pts',(0.291336800175624,1.53853171867642,-1.13937875343336));
#22986=CARTESIAN_POINT('Ctrl Pts',(0.363575843556292,2.13376828306403,0.0435672775324635));
#22987=CARTESIAN_POINT('Ctrl Pts',(0.471934408627294,1.16382771738099,1.79099441971012));
#22988=CARTESIAN_POINT('Ctrl Pts',(0.580292973698296,-0.823787078595329,
1.96871336323748));
#22989=CARTESIAN_POINT('Ctrl Pts',(0.688651538769298,-2.09121061369238,
0.428728712954709));
#22990=CARTESIAN_POINT('Ctrl Pts',(0.797010103840299,-1.53169227141652,
-1.48710898161564));
#22991=CARTESIAN_POINT('Ctrl Pts',(0.905368668911303,0.36623324217237,-2.10295184354139));
#22992=CARTESIAN_POINT('Ctrl Pts',(1.0137272339823,1.94410792168513,-0.881717409988328));
#22993=CARTESIAN_POINT('Ctrl Pts',(1.12208579905331,1.82338066158515,1.11008341380316));
#22994=CARTESIAN_POINT('Ctrl Pts',(1.23044436412431,0.109486902638216,2.13187236886589));
#22995=CARTESIAN_POINT('Ctrl Pts',(1.33880292919531,-1.70006066382498,1.29102082162132));
#22996=CARTESIAN_POINT('Ctrl Pts',(1.44716149426631,-2.02421165929592,-0.677865485064943));
#22997=CARTESIAN_POINT('Ctrl Pts',(1.55552005933731,-0.579737422444096,
-2.0544640722717));
#22998=CARTESIAN_POINT('Ctrl Pts',(1.66387862440832,1.37127200482619,-1.63601427785942));
#22999=CARTESIAN_POINT('Ctrl Pts',(1.77223718947932,2.12415481064533,0.211880809170421));
#23000=CARTESIAN_POINT('Ctrl Pts',(1.88059575455032,1.02109077962353,1.87464639961275));
#23001=CARTESIAN_POINT('Ctrl Pts',(1.98895431962132,-0.974135226807976,
1.89947051549079));
#23002=CARTESIAN_POINT('Ctrl Pts',(2.09731288469232,-2.11822561344951,0.264661584555997));
#23003=CARTESIAN_POINT('Ctrl Pts',(2.20567144976332,-1.41155078763359,-1.60139049291963));
#23004=CARTESIAN_POINT('Ctrl Pts',(2.31403001483433,0.528445927679258,-2.06825398104274));
#23005=CARTESIAN_POINT('Ctrl Pts',(2.42238857990533,2.00671802000115,-0.728011601171293));
#23006=CARTESIAN_POINT('Ctrl Pts',(2.53074714497633,1.73165846110027,1.24831623860771));
#23007=CARTESIAN_POINT('Ctrl Pts',(2.63910571004733,-0.0564225796178219,
2.13395349411699));
#23008=CARTESIAN_POINT('Ctrl Pts',(2.74746427511834,-1.79518173150733,1.15507130942012));
#23009=CARTESIAN_POINT('Ctrl Pts',(2.85582284018934,-1.96547428678394,-0.833014436030208));
#23010=CARTESIAN_POINT('Ctrl Pts',(2.96418140526034,-0.418378778651093,
-2.09330848176036));
#23011=CARTESIAN_POINT('Ctrl Pts',(3.07253997033134,1.49410415205079,-1.52452813248913));
#23012=CARTESIAN_POINT('Ctrl Pts',(3.18089853540234,2.10145146680416,0.376133048515631));
#23013=CARTESIAN_POINT('Ctrl Pts',(3.28925710047335,0.872088081817974,1.94844361419121));
#23014=CARTESIAN_POINT('Ctrl Pts',(3.39761566554435,-1.11809819681501,1.81777718099042));
#23015=CARTESIAN_POINT('Ctrl Pts',(3.50597423061535,-2.13358137239638,0.0999324498858656));
#23016=CARTESIAN_POINT('Ctrl Pts',(3.61433279568635,-1.28047295312785,-1.70741155255248));
#23017=CARTESIAN_POINT('Ctrl Pts',(3.68657183906702,0.027529040653905,-1.91428993234292));
#23018=CARTESIAN_POINT('Ctrl Pts',(3.72269136075735,0.5865088280811,-1.72413903800149));
#23019=CARTESIAN_POINT('Ctrl Pts',(0.331908639242645,0.98077109908139,-1.37424797458505));
#23020=CARTESIAN_POINT('Ctrl Pts',(0.368028160932979,1.42631338063441,-1.05627407085933));
#23021=CARTESIAN_POINT('Ctrl Pts',(0.440267204313648,1.97813422782453,0.0403895416311738));
#23022=CARTESIAN_POINT('Ctrl Pts',(0.548625769384648,1.07893976178909,1.66036180760168));
#23023=CARTESIAN_POINT('Ctrl Pts',(0.656984334455652,-0.763701208581558,
1.82511818153158));
#23024=CARTESIAN_POINT('Ctrl Pts',(0.765342899526653,-1.93868065495597,
0.39745784407717));
#23025=CARTESIAN_POINT('Ctrl Pts',(0.873701464597655,-1.41997279303096,
-1.37864134563618));
#23026=CARTESIAN_POINT('Ctrl Pts',(0.982060029668658,0.339520704969898,
-1.94956549602583));
#23027=CARTESIAN_POINT('Ctrl Pts',(1.09041859473966,1.80230742625336,-0.817406183141006));
#23028=CARTESIAN_POINT('Ctrl Pts',(1.19877715981066,1.69038584257871,1.02911549206791));
#23029=CARTESIAN_POINT('Ctrl Pts',(1.30713572488166,0.101501082065082,1.97637659893946));
#23030=CARTESIAN_POINT('Ctrl Pts',(1.41549428995266,-1.57606063187948,1.19685558003331));
#23031=CARTESIAN_POINT('Ctrl Pts',(1.52385285502367,-1.87656850999063,-0.62842293069533));
#23032=CARTESIAN_POINT('Ctrl Pts',(1.63221142009467,-0.537452190844577,
-1.90461435454492));
#23033=CARTESIAN_POINT('Ctrl Pts',(1.74056998516567,1.27125335489057,-1.51668569915951));
#23034=CARTESIAN_POINT('Ctrl Pts',(1.84892855023667,1.96922194855287,0.19642652117657));
#23035=CARTESIAN_POINT('Ctrl Pts',(1.95728711530767,0.946613855366191,1.73791232983226));
#23036=CARTESIAN_POINT('Ctrl Pts',(2.06564568037868,-0.903083174482,1.76092580963867));
#23037=CARTESIAN_POINT('Ctrl Pts',(2.17400424544968,-1.96372521865503,0.245357541095656));
#23038=CARTESIAN_POINT('Ctrl Pts',(2.28236281052068,-1.3085942599733,-1.48458732435947));
#23039=CARTESIAN_POINT('Ctrl Pts',(2.39072137559169,0.489901825513946,-1.91739844677981));
#23040=CARTESIAN_POINT('Ctrl Pts',(2.49907994066268,1.86035083212334,-0.674911459674677));
#23041=CARTESIAN_POINT('Ctrl Pts',(2.60743850573369,1.60535373029612,1.15726580919705));
#23042=CARTESIAN_POINT('Ctrl Pts',(2.71579707080469,-0.0523071960765568,
1.97830592984397));
#23043=CARTESIAN_POINT('Ctrl Pts',(2.82415563587569,-1.66424370277014,1.07082203390004));
#23044=CARTESIAN_POINT('Ctrl Pts',(2.9325142009467,-1.8221153587555,-0.772255535552851));
#23045=CARTESIAN_POINT('Ctrl Pts',(3.04087276601769,-0.387862819413889,
-1.94062550747986));
#23046=CARTESIAN_POINT('Ctrl Pts',(3.1492313310887,1.38512629818565,-1.41333119631325));
#23047=CARTESIAN_POINT('Ctrl Pts',(3.2575898961597,1.948174554656,0.348698433372686));
#23048=CARTESIAN_POINT('Ctrl Pts',(3.3659484612307,0.808479204613899,1.80632687945063));
#23049=CARTESIAN_POINT('Ctrl Pts',(3.47430702630171,-1.03654568808786,1.68519107197153));
#23050=CARTESIAN_POINT('Ctrl Pts',(3.5826655913727,-1.9779609501579,0.0926435176483781));
#23051=CARTESIAN_POINT('Ctrl Pts',(3.69102415644371,-1.18707705822139,-1.58287535712974));
#23052=CARTESIAN_POINT('Ctrl Pts',(3.76326319982438,0.0255211111763578,
-1.77466431908426));
#23053=CARTESIAN_POINT('Ctrl Pts',(3.79938272151471,0.543729699685325,-1.59838276333441));
#23054=CARTESIAN_POINT('Ctrl Pts',(0.408600000000001,0.903606778650209,
-1.26612599672283));
#23055=CARTESIAN_POINT('Ctrl Pts',(0.444719521690335,1.31409504259239,-0.973169388285302));
#23056=CARTESIAN_POINT('Ctrl Pts',(0.516958565071003,1.82250017258503,0.0372118057298887));
#23057=CARTESIAN_POINT('Ctrl Pts',(0.625317130142004,0.994051806197197,
1.52972919549323));
#23058=CARTESIAN_POINT('Ctrl Pts',(0.733675695213007,-0.703615338567789,
1.6815229998257));
#23059=CARTESIAN_POINT('Ctrl Pts',(0.842034260284009,-1.78615069621955,
0.366186975199626));
#23060=CARTESIAN_POINT('Ctrl Pts',(0.95039282535501,-1.30825331464541,-1.27017370965671));
#23061=CARTESIAN_POINT('Ctrl Pts',(1.05875139042601,0.312808167767432,-1.79617914851027));
#23062=CARTESIAN_POINT('Ctrl Pts',(1.16710995549701,1.66050693082158,-0.753094956293683));
#23063=CARTESIAN_POINT('Ctrl Pts',(1.27546852056802,1.55739102357227,0.948147570332657));
#23064=CARTESIAN_POINT('Ctrl Pts',(1.38382708563902,0.093515261491943,1.82088082901303));
#23065=CARTESIAN_POINT('Ctrl Pts',(1.49218565071002,-1.45206059993398,1.1026903384453));
#23066=CARTESIAN_POINT('Ctrl Pts',(1.60054421578102,-1.72892536068535,-0.57898037632572));
#23067=CARTESIAN_POINT('Ctrl Pts',(1.70890278085203,-0.495166959245057,
-1.75476463681813));
#23068=CARTESIAN_POINT('Ctrl Pts',(1.81726134592303,1.17123470495496,-1.39735712045959));
#23069=CARTESIAN_POINT('Ctrl Pts',(1.92561991099403,1.81428908646041,0.180972233182718));
#23070=CARTESIAN_POINT('Ctrl Pts',(2.03397847606503,0.872136931108851,1.60117826005178));
#23071=CARTESIAN_POINT('Ctrl Pts',(2.14233704113603,-0.832031122156023,
1.62238110378654));
#23072=CARTESIAN_POINT('Ctrl Pts',(2.25069560620703,-1.80922482386055,0.226053497635316));
#23073=CARTESIAN_POINT('Ctrl Pts',(2.35905417127804,-1.20563773231302,-1.3677841557993));
#23074=CARTESIAN_POINT('Ctrl Pts',(2.46741273634904,0.451357723348635,-1.76654291251687));
#23075=CARTESIAN_POINT('Ctrl Pts',(2.57577130142004,1.71398364424552,-0.621811318178061));
#23076=CARTESIAN_POINT('Ctrl Pts',(2.68412986649104,1.47904899949198,1.06621537978638));
#23077=CARTESIAN_POINT('Ctrl Pts',(2.79248843156204,-0.0481918125352924,
1.82265836557096));
#23078=CARTESIAN_POINT('Ctrl Pts',(2.90084699663305,-1.53330567403294,0.98657275837997));
#23079=CARTESIAN_POINT('Ctrl Pts',(3.00920556170405,-1.67875643072706,-0.711496635075496));
#23080=CARTESIAN_POINT('Ctrl Pts',(3.11756412677505,-0.357346860176684,
-1.78794253319936));
#23081=CARTESIAN_POINT('Ctrl Pts',(3.22592269184605,1.2761484443205,-1.30213426013737));
#23082=CARTESIAN_POINT('Ctrl Pts',(3.33428125691706,1.79489764250785,0.32126381822974));
#23083=CARTESIAN_POINT('Ctrl Pts',(3.44263982198805,0.744870327409823,1.66421014471004));
#23084=CARTESIAN_POINT('Ctrl Pts',(3.55099838705906,-0.954993179360717,
1.55260496295264));
#23085=CARTESIAN_POINT('Ctrl Pts',(3.65935695213006,-1.82234052791941,0.0853545854108896));
#23086=CARTESIAN_POINT('Ctrl Pts',(3.76771551720107,-1.09368116331493,-1.45833916170699));
#23087=CARTESIAN_POINT('Ctrl Pts',(3.83995456058173,0.0235131816988109,
-1.63503870582561));
#23088=CARTESIAN_POINT('Ctrl Pts',(3.87607408227207,0.50095057128955,-1.47262648866733));
#23089=CARTESIAN_POINT('Ctrl Pts',(3.646,0.629287956476874,-1.84989531266857));
#23090=CARTESIAN_POINT('Ctrl Pts',(3.60988047830967,0.0295369701314485,
-2.05391554560157));
#23091=CARTESIAN_POINT('Ctrl Pts',(3.57376095661933,-0.672165938951437,
-1.9429316467884));
#23092=CARTESIAN_POINT('Ctrl Pts',(3.537641434929,-1.17557288459297,-1.56424484236538));
#23093=CARTESIAN_POINT('Ctrl Pts',(3.50325085399408,-1.65488314389577,-1.20368471900189));
#23094=CARTESIAN_POINT('Ctrl Pts',(3.46886027305915,-1.95442683952169,-0.600436693209037));
#23095=CARTESIAN_POINT('Ctrl Pts',(3.43446969212423,-1.95694215816793,0.000613609334558611));
#23096=CARTESIAN_POINT('Origin',(1.705,0.,0.));
#23097=CARTESIAN_POINT('',(1.4,0.,0.));
#23098=CARTESIAN_POINT('',(2.,-0.98360655737705,1.20457062211215E-16));
#23099=CARTESIAN_POINT('',(1.705,-0.5,-6.12323399573677E-17));
#23100=CARTESIAN_POINT('Origin',(2.,0.,0.));
#23101=CARTESIAN_POINT('Origin',(2.,7.07050159149938E-17,1.15470053837925));
#23102=CARTESIAN_POINT('',(4.,-1.,0.577350269189626));
#23103=CARTESIAN_POINT('',(4.,7.07050159149938E-17,1.15470053837925));
#23104=CARTESIAN_POINT('',(4.,-0.25,1.01036297108185));
#23105=CARTESIAN_POINT('',(2.,-1.,0.577350269189626));
#23106=CARTESIAN_POINT('',(2.,-1.,0.577350269189626));
#23107=CARTESIAN_POINT('',(2.,7.07050159149938E-17,1.15470053837925));
#23108=CARTESIAN_POINT('',(2.,7.07050159149938E-17,1.15470053837925));
#23109=CARTESIAN_POINT('',(2.,7.07050159149938E-17,1.15470053837925));
#23110=CARTESIAN_POINT('Origin',(2.,1.,0.577350269189626));
#23111=CARTESIAN_POINT('',(4.,1.,0.577350269189626));
#23112=CARTESIAN_POINT('',(4.,0.75,0.721687836487032));
#23113=CARTESIAN_POINT('',(2.,1.,0.577350269189626));
#23114=CARTESIAN_POINT('',(2.,1.,0.577350269189626));
#23115=CARTESIAN_POINT('',(2.,1.,0.577350269189626));
#23116=CARTESIAN_POINT('Origin',(2.,1.,-0.577350269189626));
#23117=CARTESIAN_POINT('',(4.,1.,-0.577350269189626));
#23118=CARTESIAN_POINT('',(4.,1.,-0.288675134594813));
#23119=CARTESIAN_POINT('',(2.,1.,-0.577350269189626));
#23120=CARTESIAN_POINT('',(2.,1.,-0.577350269189626));
#23121=CARTESIAN_POINT('',(2.,1.,-0.577350269189626));
#23122=CARTESIAN_POINT('Origin',(2.,-2.12115047744981E-16,-1.15470053837925));
#23123=CARTESIAN_POINT('',(4.,-2.12115047744981E-16,-1.15470053837925));
#23124=CARTESIAN_POINT('',(4.,0.25,-1.01036297108185));
#23125=CARTESIAN_POINT('',(2.,-2.12115047744981E-16,-1.15470053837925));
#23126=CARTESIAN_POINT('',(2.,-2.12115047744981E-16,-1.15470053837925));
#23127=CARTESIAN_POINT('',(2.,-2.12115047744981E-16,-1.15470053837925));
#23128=CARTESIAN_POINT('Origin',(2.,-1.,-0.577350269189626));
#23129=CARTESIAN_POINT('',(4.,-1.,-0.577350269189626));
#23130=CARTESIAN_POINT('',(4.,-0.75,-0.721687836487032));
#23131=CARTESIAN_POINT('',(2.,-1.,-0.577350269189626));
#23132=CARTESIAN_POINT('',(2.,-1.,-0.577350269189626));
#23133=CARTESIAN_POINT('',(2.,-1.,-0.577350269189626));
#23134=CARTESIAN_POINT('Origin',(2.,-1.,0.577350269189626));
#23135=CARTESIAN_POINT('',(4.,-1.,0.288675134594813));
#23136=CARTESIAN_POINT('',(2.,-1.,0.577350269189626));
#23137=CARTESIAN_POINT('Origin',(2.,0.,0.));
#23138=CARTESIAN_POINT('Origin',(0.,1.5,0.));
#23139=CARTESIAN_POINT('',(1.04083408558608E-16,-1.5,-1.83697019872103E-16));
#23140=CARTESIAN_POINT('Origin',(0.,0.,0.));
#23141=CARTESIAN_POINT('Origin',(0.225,0.,0.));
#23142=CARTESIAN_POINT('',(0.225,-1.75,-2.14313189850787E-16));
#23143=CARTESIAN_POINT('Origin',(2.025,0.,0.));
#23144=CARTESIAN_POINT('Origin',(3.646,0.,0.));
#23145=CARTESIAN_POINT('Origin',(3.8,0.,0.));
#23146=CARTESIAN_POINT('',(4.,-1.6,-1.95943487863577E-16));
#23147=CARTESIAN_POINT('Origin',(4.,0.,0.));
#23148=CARTESIAN_POINT('',(3.8,-1.8,-2.20436423846524E-16));
#23149=CARTESIAN_POINT('Origin',(4.,0.,0.));
#23150=CARTESIAN_POINT('',(0.,0.,0.));
#23151=CARTESIAN_POINT('Origin',(0.,11.3,3.6));
#23152=CARTESIAN_POINT('',(0.,11.3,4.45));
#23153=CARTESIAN_POINT('Origin',(0.,11.3,3.6));
#23154=CARTESIAN_POINT('',(1.2,11.3,4.45));
#23155=CARTESIAN_POINT('',(0.,11.3,4.45));
#23156=CARTESIAN_POINT('Origin',(1.2,11.3,3.6));
#23157=CARTESIAN_POINT('Origin',(0.,11.3,-3.6));
#23158=CARTESIAN_POINT('',(0.,11.3,-2.75));
#23159=CARTESIAN_POINT('Origin',(0.,11.3,-3.6));
#23160=CARTESIAN_POINT('',(1.2,11.3,-2.75));
#23161=CARTESIAN_POINT('',(0.,11.3,-2.75));
#23162=CARTESIAN_POINT('Origin',(1.2,11.3,-3.6));
#23163=CARTESIAN_POINT('Origin',(0.6,0.,0.));
#23164=CARTESIAN_POINT('',(1.2,14.5633100633063,2.));
#23165=CARTESIAN_POINT('',(0.,14.5633100633063,2.));
#23166=CARTESIAN_POINT('',(0.6,14.5633100633063,2.));
#23167=CARTESIAN_POINT('',(0.,14.5633100633063,-2.));
#23168=CARTESIAN_POINT('Origin',(0.,0.,0.));
#23169=CARTESIAN_POINT('',(1.2,14.5633100633063,-2.));
#23170=CARTESIAN_POINT('',(0.6,14.5633100633063,-2.));
#23171=CARTESIAN_POINT('Origin',(1.2,0.,0.));
#23172=CARTESIAN_POINT('Origin',(0.,14.7,0.));
#23173=CARTESIAN_POINT('',(0.,10.2,2.));
#23174=CARTESIAN_POINT('',(0.,10.2,2.));
#23175=CARTESIAN_POINT('',(0.,10.2,5.));
#23176=CARTESIAN_POINT('',(0.,10.2,5.));
#23177=CARTESIAN_POINT('',(0.,11.3472463620034,5.));
#23178=CARTESIAN_POINT('',(0.,12.6,5.));
#23179=CARTESIAN_POINT('',(0.,11.3472463620034,-5.));
#23180=CARTESIAN_POINT('Origin',(0.,0.,0.));
#23181=CARTESIAN_POINT('',(0.,10.2,-5.));
#23182=CARTESIAN_POINT('',(0.,12.6,-5.));
#23183=CARTESIAN_POINT('',(0.,10.2,-2.));
#23184=CARTESIAN_POINT('',(0.,10.2,-5.));
#23185=CARTESIAN_POINT('',(0.,12.1,-2.));
#23186=CARTESIAN_POINT('Origin',(0.,10.2,-5.));
#23187=CARTESIAN_POINT('',(1.2,11.3472463620034,-5.));
#23188=CARTESIAN_POINT('',(0.6,11.3472463620034,-5.));
#23189=CARTESIAN_POINT('',(1.2,10.2,-5.));
#23190=CARTESIAN_POINT('',(1.2,12.6,-5.));
#23191=CARTESIAN_POINT('',(0.,10.2,-5.));
#23192=CARTESIAN_POINT('Origin',(0.,10.2,-2.));
#23193=CARTESIAN_POINT('',(1.2,10.2,-2.));
#23194=CARTESIAN_POINT('',(1.2,10.2,-5.));
#23195=CARTESIAN_POINT('',(0.,10.2,-2.));
#23196=CARTESIAN_POINT('Origin',(0.,12.6,-2.));
#23197=CARTESIAN_POINT('',(1.2,10.95,-2.));
#23198=CARTESIAN_POINT('Origin',(0.,10.2,2.));
#23199=CARTESIAN_POINT('',(1.2,10.2,2.));
#23200=CARTESIAN_POINT('',(1.2,13.95,2.));
#23201=CARTESIAN_POINT('',(0.,10.2,2.));
#23202=CARTESIAN_POINT('Origin',(0.,12.6,5.));
#23203=CARTESIAN_POINT('',(1.2,11.3472463620034,5.));
#23204=CARTESIAN_POINT('',(0.6,11.3472463620034,5.));
#23205=CARTESIAN_POINT('',(1.2,10.2,5.));
#23206=CARTESIAN_POINT('',(0.,10.2,5.));
#23207=CARTESIAN_POINT('',(1.2,12.6,5.));
#23208=CARTESIAN_POINT('Origin',(0.,10.2,5.));
#23209=CARTESIAN_POINT('',(1.2,10.2,5.));
#23210=CARTESIAN_POINT('Origin',(1.2,12.4,0.));
#23211=CARTESIAN_POINT('Origin',(1.2,0.,0.));
#23212=CARTESIAN_POINT('Origin',(0.6,0.,0.));
#23213=CARTESIAN_POINT('',(0.,0.,0.));
#23214=CARTESIAN_POINT('',(0.,0.,55.));
#23215=CARTESIAN_POINT('',(0.,0.,55.));
#23216=CARTESIAN_POINT('',(0.,0.,55.));
#23217=CARTESIAN_POINT('',(0.,0.,55.));
#23218=CARTESIAN_POINT('',(0.,30.,55.));
#23219=CARTESIAN_POINT('',(0.,52.,55.));
#23220=CARTESIAN_POINT('',(30.,0.,55.));
#23221=CARTESIAN_POINT('',(-30.,0.,55.));
#23222=CARTESIAN_POINT('',(29.45,0.,55.));
#23223=CARTESIAN_POINT('',(0.,29.45,55.));
#23224=CARTESIAN_POINT('',(24.5,0.,60.5));
#23225=CARTESIAN_POINT('',(24.5,-5.5,55.));
#23226=CARTESIAN_POINT('',(0.,24.5,49.5));
#23227=CARTESIAN_POINT('',(-5.5,24.5,55.));
#23228=CARTESIAN_POINT('',(38.,0.,55.));
#23229=CARTESIAN_POINT('',(-38.,0.,55.));
#23230=CARTESIAN_POINT('',(0.,52.,55.));
#23231=UNCERTAINTY_MEASURE_WITH_UNIT(LENGTH_MEASURE(0.01),#23255,
'DISTANCE_ACCURACY_VALUE',
'Maximum model space distance between geometric entities at asserted c
onnectivities');
#23232=UNCERTAINTY_MEASURE_WITH_UNIT(LENGTH_MEASURE(0.01),#23255,
'DISTANCE_ACCURACY_VALUE',
'Maximum model space distance between geometric entities at asserted c
onnectivities');
#23233=UNCERTAINTY_MEASURE_WITH_UNIT(LENGTH_MEASURE(0.01),#23255,
'DISTANCE_ACCURACY_VALUE',
'Maximum model space distance between geometric entities at asserted c
onnectivities');
#23234=UNCERTAINTY_MEASURE_WITH_UNIT(LENGTH_MEASURE(0.01),#23255,
'DISTANCE_ACCURACY_VALUE',
'Maximum model space distance between geometric entities at asserted c
onnectivities');
#23235=UNCERTAINTY_MEASURE_WITH_UNIT(LENGTH_MEASURE(0.01),#23255,
'DISTANCE_ACCURACY_VALUE',
'Maximum model space distance between geometric entities at asserted c
onnectivities');
#23236=UNCERTAINTY_MEASURE_WITH_UNIT(LENGTH_MEASURE(0.01),#23255,
'DISTANCE_ACCURACY_VALUE',
'Maximum model space distance between geometric entities at asserted c
onnectivities');
#23237=UNCERTAINTY_MEASURE_WITH_UNIT(LENGTH_MEASURE(0.01),#23255,
'DISTANCE_ACCURACY_VALUE',
'Maximum model space distance between geometric entities at asserted c
onnectivities');
#23238=UNCERTAINTY_MEASURE_WITH_UNIT(LENGTH_MEASURE(0.01),#23255,
'DISTANCE_ACCURACY_VALUE',
'Maximum model space distance between geometric entities at asserted c
onnectivities');
#23239=UNCERTAINTY_MEASURE_WITH_UNIT(LENGTH_MEASURE(0.01),#23255,
'DISTANCE_ACCURACY_VALUE',
'Maximum model space distance between geometric entities at asserted c
onnectivities');
#23240=UNCERTAINTY_MEASURE_WITH_UNIT(LENGTH_MEASURE(0.01),#23255,
'DISTANCE_ACCURACY_VALUE',
'Maximum model space distance between geometric entities at asserted c
onnectivities');
#23241=UNCERTAINTY_MEASURE_WITH_UNIT(LENGTH_MEASURE(0.01),#23255,
'DISTANCE_ACCURACY_VALUE',
'Maximum model space distance between geometric entities at asserted c
onnectivities');
#23242=UNCERTAINTY_MEASURE_WITH_UNIT(LENGTH_MEASURE(0.01),#23255,
'DISTANCE_ACCURACY_VALUE',
'Maximum model space distance between geometric entities at asserted c
onnectivities');
#23243=(
GEOMETRIC_REPRESENTATION_CONTEXT(3)
GLOBAL_UNCERTAINTY_ASSIGNED_CONTEXT((#23231))
GLOBAL_UNIT_ASSIGNED_CONTEXT((#23255,#23257,#23258))
REPRESENTATION_CONTEXT('','3D')
);
#23244=(
GEOMETRIC_REPRESENTATION_CONTEXT(3)
GLOBAL_UNCERTAINTY_ASSIGNED_CONTEXT((#23232))
GLOBAL_UNIT_ASSIGNED_CONTEXT((#23255,#23257,#23258))
REPRESENTATION_CONTEXT('','3D')
);
#23245=(
GEOMETRIC_REPRESENTATION_CONTEXT(3)
GLOBAL_UNCERTAINTY_ASSIGNED_CONTEXT((#23233))
GLOBAL_UNIT_ASSIGNED_CONTEXT((#23255,#23257,#23258))
REPRESENTATION_CONTEXT('','3D')
);
#23246=(
GEOMETRIC_REPRESENTATION_CONTEXT(3)
GLOBAL_UNCERTAINTY_ASSIGNED_CONTEXT((#23234))
GLOBAL_UNIT_ASSIGNED_CONTEXT((#23255,#23257,#23258))
REPRESENTATION_CONTEXT('','3D')
);
#23247=(
GEOMETRIC_REPRESENTATION_CONTEXT(3)
GLOBAL_UNCERTAINTY_ASSIGNED_CONTEXT((#23235))
GLOBAL_UNIT_ASSIGNED_CONTEXT((#23255,#23257,#23258))
REPRESENTATION_CONTEXT('','3D')
);
#23248=(
GEOMETRIC_REPRESENTATION_CONTEXT(3)
GLOBAL_UNCERTAINTY_ASSIGNED_CONTEXT((#23236))
GLOBAL_UNIT_ASSIGNED_CONTEXT((#23255,#23257,#23258))
REPRESENTATION_CONTEXT('','3D')
);
#23249=(
GEOMETRIC_REPRESENTATION_CONTEXT(3)
GLOBAL_UNCERTAINTY_ASSIGNED_CONTEXT((#23237))
GLOBAL_UNIT_ASSIGNED_CONTEXT((#23255,#23257,#23258))
REPRESENTATION_CONTEXT('','3D')
);
#23250=(
GEOMETRIC_REPRESENTATION_CONTEXT(3)
GLOBAL_UNCERTAINTY_ASSIGNED_CONTEXT((#23238))
GLOBAL_UNIT_ASSIGNED_CONTEXT((#23255,#23257,#23258))
REPRESENTATION_CONTEXT('','3D')
);
#23251=(
GEOMETRIC_REPRESENTATION_CONTEXT(3)
GLOBAL_UNCERTAINTY_ASSIGNED_CONTEXT((#23239))
GLOBAL_UNIT_ASSIGNED_CONTEXT((#23255,#23257,#23258))
REPRESENTATION_CONTEXT('','3D')
);
#23252=(
GEOMETRIC_REPRESENTATION_CONTEXT(3)
GLOBAL_UNCERTAINTY_ASSIGNED_CONTEXT((#23240))
GLOBAL_UNIT_ASSIGNED_CONTEXT((#23255,#23257,#23258))
REPRESENTATION_CONTEXT('','3D')
);
#23253=(
GEOMETRIC_REPRESENTATION_CONTEXT(3)
GLOBAL_UNCERTAINTY_ASSIGNED_CONTEXT((#23241))
GLOBAL_UNIT_ASSIGNED_CONTEXT((#23255,#23257,#23258))
REPRESENTATION_CONTEXT('','3D')
);
#23254=(
GEOMETRIC_REPRESENTATION_CONTEXT(3)
GLOBAL_UNCERTAINTY_ASSIGNED_CONTEXT((#23242))
GLOBAL_UNIT_ASSIGNED_CONTEXT((#23255,#23257,#23258))
REPRESENTATION_CONTEXT('','3D')
);
#23255=(
LENGTH_UNIT()
NAMED_UNIT(*)
SI_UNIT(.MILLI.,.METRE.)
);
#23256=(
LENGTH_UNIT()
NAMED_UNIT(*)
SI_UNIT($,.METRE.)
);
#23257=(
NAMED_UNIT(*)
PLANE_ANGLE_UNIT()
SI_UNIT($,.RADIAN.)
);
#23258=(
NAMED_UNIT(*)
SI_UNIT($,.STERADIAN.)
SOLID_ANGLE_UNIT()
);
#23259=SHAPE_DEFINITION_REPRESENTATION(#23270,#23299);
#23260=SHAPE_DEFINITION_REPRESENTATION(#23271,#23300);
#23261=SHAPE_DEFINITION_REPRESENTATION(#23272,#23301);
#23262=SHAPE_DEFINITION_REPRESENTATION(#23273,#23302);
#23263=SHAPE_DEFINITION_REPRESENTATION(#23274,#23303);
#23264=SHAPE_DEFINITION_REPRESENTATION(#23275,#23304);
#23265=SHAPE_DEFINITION_REPRESENTATION(#23276,#23305);
#23266=SHAPE_DEFINITION_REPRESENTATION(#23277,#23306);
#23267=SHAPE_DEFINITION_REPRESENTATION(#23278,#23307);
#23268=SHAPE_DEFINITION_REPRESENTATION(#23279,#23308);
#23269=SHAPE_DEFINITION_REPRESENTATION(#23280,#23309);
#23270=PRODUCT_DEFINITION_SHAPE('',$,#23311);
#23271=PRODUCT_DEFINITION_SHAPE('',$,#23312);
#23272=PRODUCT_DEFINITION_SHAPE('',$,#23313);
#23273=PRODUCT_DEFINITION_SHAPE('',$,#23314);
#23274=PRODUCT_DEFINITION_SHAPE('',$,#23315);
#23275=PRODUCT_DEFINITION_SHAPE('',$,#23316);
#23276=PRODUCT_DEFINITION_SHAPE('',$,#23317);
#23277=PRODUCT_DEFINITION_SHAPE('',$,#23318);
#23278=PRODUCT_DEFINITION_SHAPE('',$,#23319);
#23279=PRODUCT_DEFINITION_SHAPE('',$,#23320);
#23280=PRODUCT_DEFINITION_SHAPE('',$,#23321);
#23281=PRODUCT_DEFINITION_SHAPE($,$,#65);
#23282=PRODUCT_DEFINITION_SHAPE($,$,#66);
#23283=PRODUCT_DEFINITION_SHAPE($,$,#67);
#23284=PRODUCT_DEFINITION_SHAPE($,$,#68);
#23285=PRODUCT_DEFINITION_SHAPE($,$,#69);
#23286=PRODUCT_DEFINITION_SHAPE($,$,#70);
#23287=PRODUCT_DEFINITION_SHAPE($,$,#71);
#23288=PRODUCT_DEFINITION_SHAPE($,$,#72);
#23289=PRODUCT_DEFINITION_SHAPE($,$,#73);
#23290=PRODUCT_DEFINITION_SHAPE($,$,#74);
#23291=PRODUCT_DEFINITION_SHAPE($,$,#75);
#23292=PRODUCT_DEFINITION_SHAPE($,$,#76);
#23293=PRODUCT_DEFINITION_SHAPE($,$,#77);
#23294=PRODUCT_DEFINITION_SHAPE($,$,#78);
#23295=PRODUCT_DEFINITION_SHAPE($,$,#79);
#23296=PRODUCT_DEFINITION_SHAPE($,$,#80);
#23297=PRODUCT_DEFINITION_SHAPE($,$,#81);
#23298=PRODUCT_DEFINITION_SHAPE($,$,#82);
#23299=SHAPE_REPRESENTATION('',(#7146,#7813,#7814,#7815,#7816,#7817,#7818,
#7819,#7820,#7821,#7822,#7823,#7824,#7825,#7826,#7827,#7828,#7829,#7830),
#23243);
#23300=SHAPE_REPRESENTATION('',(#7147),#23244);
#23301=SHAPE_REPRESENTATION('',(#7279),#23245);
#23302=SHAPE_REPRESENTATION('',(#7412),#23246);
#23303=SHAPE_REPRESENTATION('',(#7544),#23247);
#23304=SHAPE_REPRESENTATION('',(#7574),#23248);
#23305=SHAPE_REPRESENTATION('',(#7604),#23249);
#23306=SHAPE_REPRESENTATION('',(#7713),#23250);
#23307=SHAPE_REPRESENTATION('',(#7746),#23251);
#23308=SHAPE_REPRESENTATION('',(#7755),#23252);
#23309=SHAPE_REPRESENTATION('',(#7792),#23253);
#23310=PRODUCT_DEFINITION_CONTEXT('part definition',#23345,'design');
#23311=PRODUCT_DEFINITION('2026-10-11-09-11-47-303','MAS-365',#23322,
#23310);
#23312=PRODUCT_DEFINITION('2026-10-11-09-11-47-549',
'01_Aluminium_Gearbox_Block_Front_Window',#23323,#23310);
#23313=PRODUCT_DEFINITION('2026-10-11-09-11-48-335',
'02_Spiral_Bevel_Input_Pinion_M1.5_Z20_LH',#23324,#23310);
#23314=PRODUCT_DEFINITION('2026-10-11-09-11-49-846',
'03_Spiral_Bevel_Output_Gear_M1.5_Z20_RH',#23325,#23310);
#23315=PRODUCT_DEFINITION('2026-10-11-09-11-51-553',
'04_Input_Shaft_D12x75',#23326,#23310);
#23316=PRODUCT_DEFINITION('2026-10-11-09-11-52-446',
'05_Output_Through_Shaft_D12x180',#23327,#23310);
#23317=PRODUCT_DEFINITION('2026-10-11-09-11-53-414',
'06_Angular_Contact_Ball_Bearing_7001_12x28x8',#23328,#23310);
#23318=PRODUCT_DEFINITION('2026-10-11-09-11-54-369',
'07_Deep_Groove_Ball_Bearing_6001-2RS_12x28x8',#23329,#23310);
#23319=PRODUCT_DEFINITION('2026-10-11-09-11-54-876',
'08_DIN_988_Shim_Washer_12x18x0.5',#23330,#23310);
#23320=PRODUCT_DEFINITION('2026-10-11-09-11-55-273',
'09_ISO_4026_M4x4_Set_Screw',#23331,#23310);
#23321=PRODUCT_DEFINITION('2026-10-11-09-11-56-293',
'10_DIN_472_28x1.2_Internal_Circlip',#23332,#23310);
#23322=PRODUCT_DEFINITION_FORMATION('',$,#23347);
#23323=PRODUCT_DEFINITION_FORMATION('',$,#23348);
#23324=PRODUCT_DEFINITION_FORMATION('',$,#23349);
#23325=PRODUCT_DEFINITION_FORMATION('',$,#23350);
#23326=PRODUCT_DEFINITION_FORMATION('',$,#23351);
#23327=PRODUCT_DEFINITION_FORMATION('',$,#23352);
#23328=PRODUCT_DEFINITION_FORMATION('',$,#23353);
#23329=PRODUCT_DEFINITION_FORMATION('',$,#23354);
#23330=PRODUCT_DEFINITION_FORMATION('',$,#23355);
#23331=PRODUCT_DEFINITION_FORMATION('',$,#23356);
#23332=PRODUCT_DEFINITION_FORMATION('',$,#23357);
#23333=PRODUCT_RELATED_PRODUCT_CATEGORY('MAS-365','MAS-365',(#23347));
#23334=PRODUCT_RELATED_PRODUCT_CATEGORY(
'01_Aluminium_Gearbox_Block_Front_Window',
'01_Aluminium_Gearbox_Block_Front_Window',(#23348));
#23335=PRODUCT_RELATED_PRODUCT_CATEGORY(
'02_Spiral_Bevel_Input_Pinion_M1.5_Z20_LH',
'02_Spiral_Bevel_Input_Pinion_M1.5_Z20_LH',(#23349));
#23336=PRODUCT_RELATED_PRODUCT_CATEGORY(
'03_Spiral_Bevel_Output_Gear_M1.5_Z20_RH',
'03_Spiral_Bevel_Output_Gear_M1.5_Z20_RH',(#23350));
#23337=PRODUCT_RELATED_PRODUCT_CATEGORY('04_Input_Shaft_D12x75',
'04_Input_Shaft_D12x75',(#23351));
#23338=PRODUCT_RELATED_PRODUCT_CATEGORY(
'05_Output_Through_Shaft_D12x180','05_Output_Through_Shaft_D12x180',(#23352));
#23339=PRODUCT_RELATED_PRODUCT_CATEGORY(
'06_Angular_Contact_Ball_Bearing_7001_12x28x8',
'06_Angular_Contact_Ball_Bearing_7001_12x28x8',(#23353));
#23340=PRODUCT_RELATED_PRODUCT_CATEGORY(
'07_Deep_Groove_Ball_Bearing_6001-2RS_12x28x8',
'07_Deep_Groove_Ball_Bearing_6001-2RS_12x28x8',(#23354));
#23341=PRODUCT_RELATED_PRODUCT_CATEGORY(
'08_DIN_988_Shim_Washer_12x18x0.5','08_DIN_988_Shim_Washer_12x18x0.5',(#23355));
#23342=PRODUCT_RELATED_PRODUCT_CATEGORY('09_ISO_4026_M4x4_Set_Screw',
'09_ISO_4026_M4x4_Set_Screw',(#23356));
#23343=PRODUCT_RELATED_PRODUCT_CATEGORY(
'10_DIN_472_28x1.2_Internal_Circlip',
'10_DIN_472_28x1.2_Internal_Circlip',(#23357));
#23344=APPLICATION_PROTOCOL_DEFINITION('international standard',
'automotive_design',2009,#23345);
#23345=APPLICATION_CONTEXT(
'Core Data for Automotive Mechanical Design Process');
#23346=PRODUCT_CONTEXT('part definition',#23345,'mechanical');
#23347=PRODUCT('2026-10-11-09-11-47-303','MAS-365',$,(#23346));
#23348=PRODUCT('2026-10-11-09-11-47-549',
'01_Aluminium_Gearbox_Block_Front_Window',$,(#23346));
#23349=PRODUCT('2026-10-11-09-11-48-335',
'02_Spiral_Bevel_Input_Pinion_M1.5_Z20_LH',$,(#23346));
#23350=PRODUCT('2026-10-11-09-11-49-846',
'03_Spiral_Bevel_Output_Gear_M1.5_Z20_RH',$,(#23346));
#23351=PRODUCT('2026-10-11-09-11-51-553','04_Input_Shaft_D12x75',$,(#23346));
#23352=PRODUCT('2026-10-11-09-11-52-446',
'05_Output_Through_Shaft_D12x180',$,(#23346));
#23353=PRODUCT('2026-10-11-09-11-53-414',
'06_Angular_Contact_Ball_Bearing_7001_12x28x8',$,(#23346));
#23354=PRODUCT('2026-10-11-09-11-54-369',
'07_Deep_Groove_Ball_Bearing_6001-2RS_12x28x8',$,(#23346));
#23355=PRODUCT('2026-10-11-09-11-54-876',
'08_DIN_988_Shim_Washer_12x18x0.5',$,(#23346));
#23356=PRODUCT('2026-10-11-09-11-55-273','09_ISO_4026_M4x4_Set_Screw',$,
(#23346));
#23357=PRODUCT('2026-10-11-09-11-56-293',
'10_DIN_472_28x1.2_Internal_Circlip',$,(#23346));
#23358=PRESENTATION_STYLE_ASSIGNMENT((#23369));
#23359=PRESENTATION_STYLE_ASSIGNMENT((#23370));
#23360=PRESENTATION_STYLE_ASSIGNMENT((#23371));
#23361=PRESENTATION_STYLE_ASSIGNMENT((#23372));
#23362=PRESENTATION_STYLE_ASSIGNMENT((#23373));
#23363=PRESENTATION_STYLE_ASSIGNMENT((#23374));
#23364=PRESENTATION_STYLE_ASSIGNMENT((#23375));
#23365=PRESENTATION_STYLE_ASSIGNMENT((#23376));
#23366=PRESENTATION_STYLE_ASSIGNMENT((#23377));
#23367=PRESENTATION_STYLE_ASSIGNMENT((#23378));
#23368=PRESENTATION_STYLE_ASSIGNMENT((#23379));
#23369=SURFACE_STYLE_USAGE(.BOTH.,#23380);
#23370=SURFACE_STYLE_USAGE(.BOTH.,#23381);
#23371=SURFACE_STYLE_USAGE(.BOTH.,#23382);
#23372=SURFACE_STYLE_USAGE(.BOTH.,#23383);
#23373=SURFACE_STYLE_USAGE(.BOTH.,#23384);
#23374=SURFACE_STYLE_USAGE(.BOTH.,#23385);
#23375=SURFACE_STYLE_USAGE(.BOTH.,#23386);
#23376=SURFACE_STYLE_USAGE(.BOTH.,#23387);
#23377=SURFACE_STYLE_USAGE(.BOTH.,#23388);
#23378=SURFACE_STYLE_USAGE(.BOTH.,#23389);
#23379=SURFACE_STYLE_USAGE(.BOTH.,#23390);
#23380=SURFACE_SIDE_STYLE('',(#23391));
#23381=SURFACE_SIDE_STYLE('',(#23392));
#23382=SURFACE_SIDE_STYLE('',(#23393));
#23383=SURFACE_SIDE_STYLE('',(#23394));
#23384=SURFACE_SIDE_STYLE('',(#23395));
#23385=SURFACE_SIDE_STYLE('',(#23396));
#23386=SURFACE_SIDE_STYLE('',(#23397));
#23387=SURFACE_SIDE_STYLE('',(#23398));
#23388=SURFACE_SIDE_STYLE('',(#23399));
#23389=SURFACE_SIDE_STYLE('',(#23400));
#23390=SURFACE_SIDE_STYLE('',(#23401));
#23391=SURFACE_STYLE_FILL_AREA(#23402);
#23392=SURFACE_STYLE_FILL_AREA(#23403);
#23393=SURFACE_STYLE_FILL_AREA(#23404);
#23394=SURFACE_STYLE_FILL_AREA(#23405);
#23395=SURFACE_STYLE_FILL_AREA(#23406);
#23396=SURFACE_STYLE_FILL_AREA(#23407);
#23397=SURFACE_STYLE_FILL_AREA(#23408);
#23398=SURFACE_STYLE_FILL_AREA(#23409);
#23399=SURFACE_STYLE_FILL_AREA(#23410);
#23400=SURFACE_STYLE_FILL_AREA(#23411);
#23401=SURFACE_STYLE_FILL_AREA(#23412);
#23402=FILL_AREA_STYLE('Steel - Satin',(#23413));
#23403=FILL_AREA_STYLE('MAS365_housing',(#23414));
#23404=FILL_AREA_STYLE('MAS365_pinion',(#23415));
#23405=FILL_AREA_STYLE('MAS365_wheel',(#23416));
#23406=FILL_AREA_STYLE('MAS365_inshaft',(#23417));
#23407=FILL_AREA_STYLE('MAS365_outshaft',(#23418));
#23408=FILL_AREA_STYLE('MAS365_b7001',(#23419));
#23409=FILL_AREA_STYLE('MAS365_b6001',(#23420));
#23410=FILL_AREA_STYLE('MAS365_shim',(#23421));
#23411=FILL_AREA_STYLE('MAS365_setscr',(#23422));
#23412=FILL_AREA_STYLE('MAS365_clip',(#23423));
#23413=FILL_AREA_STYLE_COLOUR('Steel - Satin',#23424);
#23414=FILL_AREA_STYLE_COLOUR('MAS365_housing',#23425);
#23415=FILL_AREA_STYLE_COLOUR('MAS365_pinion',#23426);
#23416=FILL_AREA_STYLE_COLOUR('MAS365_wheel',#23427);
#23417=FILL_AREA_STYLE_COLOUR('MAS365_inshaft',#23428);
#23418=FILL_AREA_STYLE_COLOUR('MAS365_outshaft',#23429);
#23419=FILL_AREA_STYLE_COLOUR('MAS365_b7001',#23430);
#23420=FILL_AREA_STYLE_COLOUR('MAS365_b6001',#23431);
#23421=FILL_AREA_STYLE_COLOUR('MAS365_shim',#23432);
#23422=FILL_AREA_STYLE_COLOUR('MAS365_setscr',#23433);
#23423=FILL_AREA_STYLE_COLOUR('MAS365_clip',#23434);
#23424=COLOUR_RGB('Steel - Satin',0.627450980392157,0.627450980392157,0.627450980392157);
#23425=COLOUR_RGB('MAS365_housing',0.768627450980392,0.776470588235294,
0.792156862745098);
#23426=COLOUR_RGB('MAS365_pinion',0.227450980392157,0.227450980392157,0.243137254901961);
#23427=COLOUR_RGB('MAS365_wheel',0.227450980392157,0.227450980392157,0.243137254901961);
#23428=COLOUR_RGB('MAS365_inshaft',0.8,0.811764705882353,0.831372549019608);
#23429=COLOUR_RGB('MAS365_outshaft',0.8,0.811764705882353,0.831372549019608);
#23430=COLOUR_RGB('MAS365_b7001',0.313725490196078,0.313725490196078,0.329411764705882);
#23431=COLOUR_RGB('MAS365_b6001',0.313725490196078,0.313725490196078,0.329411764705882);
#23432=COLOUR_RGB('MAS365_shim',0.784313725490196,0.792156862745098,0.807843137254902);
#23433=COLOUR_RGB('MAS365_setscr',0.768627450980392,0.776470588235294,0.792156862745098);
#23434=COLOUR_RGB('MAS365_clip',0.588235294117647,0.596078431372549,0.611764705882353);
#23435=COLOUR_RGB('Dark Blue',0.08,0.2,0.34);
#23436=FILL_AREA_STYLE_COLOUR('',#23435);
#23437=FILL_AREA_STYLE('',(#23436));
#23438=SURFACE_STYLE_FILL_AREA(#23437);
#23439=SURFACE_SIDE_STYLE('',(#23438));
#23440=SURFACE_STYLE_USAGE(.BOTH.,#23439);
#23441=PRESENTATION_STYLE_ASSIGNMENT((#23440));
#23442=COLOUR_RGB('Light Blue',0.38,0.62,0.78);
#23443=FILL_AREA_STYLE_COLOUR('',#23442);
#23444=FILL_AREA_STYLE('',(#23443));
#23445=SURFACE_STYLE_FILL_AREA(#23444);
#23446=SURFACE_SIDE_STYLE('',(#23445));
#23447=SURFACE_STYLE_USAGE(.BOTH.,#23446);
#23448=PRESENTATION_STYLE_ASSIGNMENT((#23447));
#23449=COLOUR_RGB('Sky Blue',0.24,0.69,0.87);
#23450=FILL_AREA_STYLE_COLOUR('',#23449);
#23451=FILL_AREA_STYLE('',(#23450));
#23452=SURFACE_STYLE_FILL_AREA(#23451);
#23453=SURFACE_SIDE_STYLE('',(#23452));
#23454=SURFACE_STYLE_USAGE(.BOTH.,#23453);
#23455=PRESENTATION_STYLE_ASSIGNMENT((#23454));
#23456=COLOUR_RGB('Grey',0.48,0.52,0.57);
#23457=FILL_AREA_STYLE_COLOUR('',#23456);
#23458=FILL_AREA_STYLE('',(#23457));
#23459=SURFACE_STYLE_FILL_AREA(#23458);
#23460=SURFACE_SIDE_STYLE('',(#23459));
#23461=SURFACE_STYLE_USAGE(.BOTH.,#23460);
#23462=PRESENTATION_STYLE_ASSIGNMENT((#23461));
#23463=COLOUR_RGB('Black',0.12,0.14,0.17);
#23464=FILL_AREA_STYLE_COLOUR('',#23463);
#23465=FILL_AREA_STYLE('',(#23464));
#23466=SURFACE_STYLE_FILL_AREA(#23465);
#23467=SURFACE_SIDE_STYLE('',(#23466));
#23468=SURFACE_STYLE_USAGE(.BOTH.,#23467);
#23469=PRESENTATION_STYLE_ASSIGNMENT((#23468));
#23470=COLOUR_RGB('Off White',0.89,0.88,0.83);
#23471=FILL_AREA_STYLE_COLOUR('',#23470);
#23472=FILL_AREA_STYLE('',(#23471));
#23473=SURFACE_STYLE_FILL_AREA(#23472);
#23474=SURFACE_SIDE_STYLE('',(#23473));
#23475=SURFACE_STYLE_USAGE(.BOTH.,#23474);
#23476=PRESENTATION_STYLE_ASSIGNMENT((#23475));
ENDSEC;
END-ISO-10303-21;
